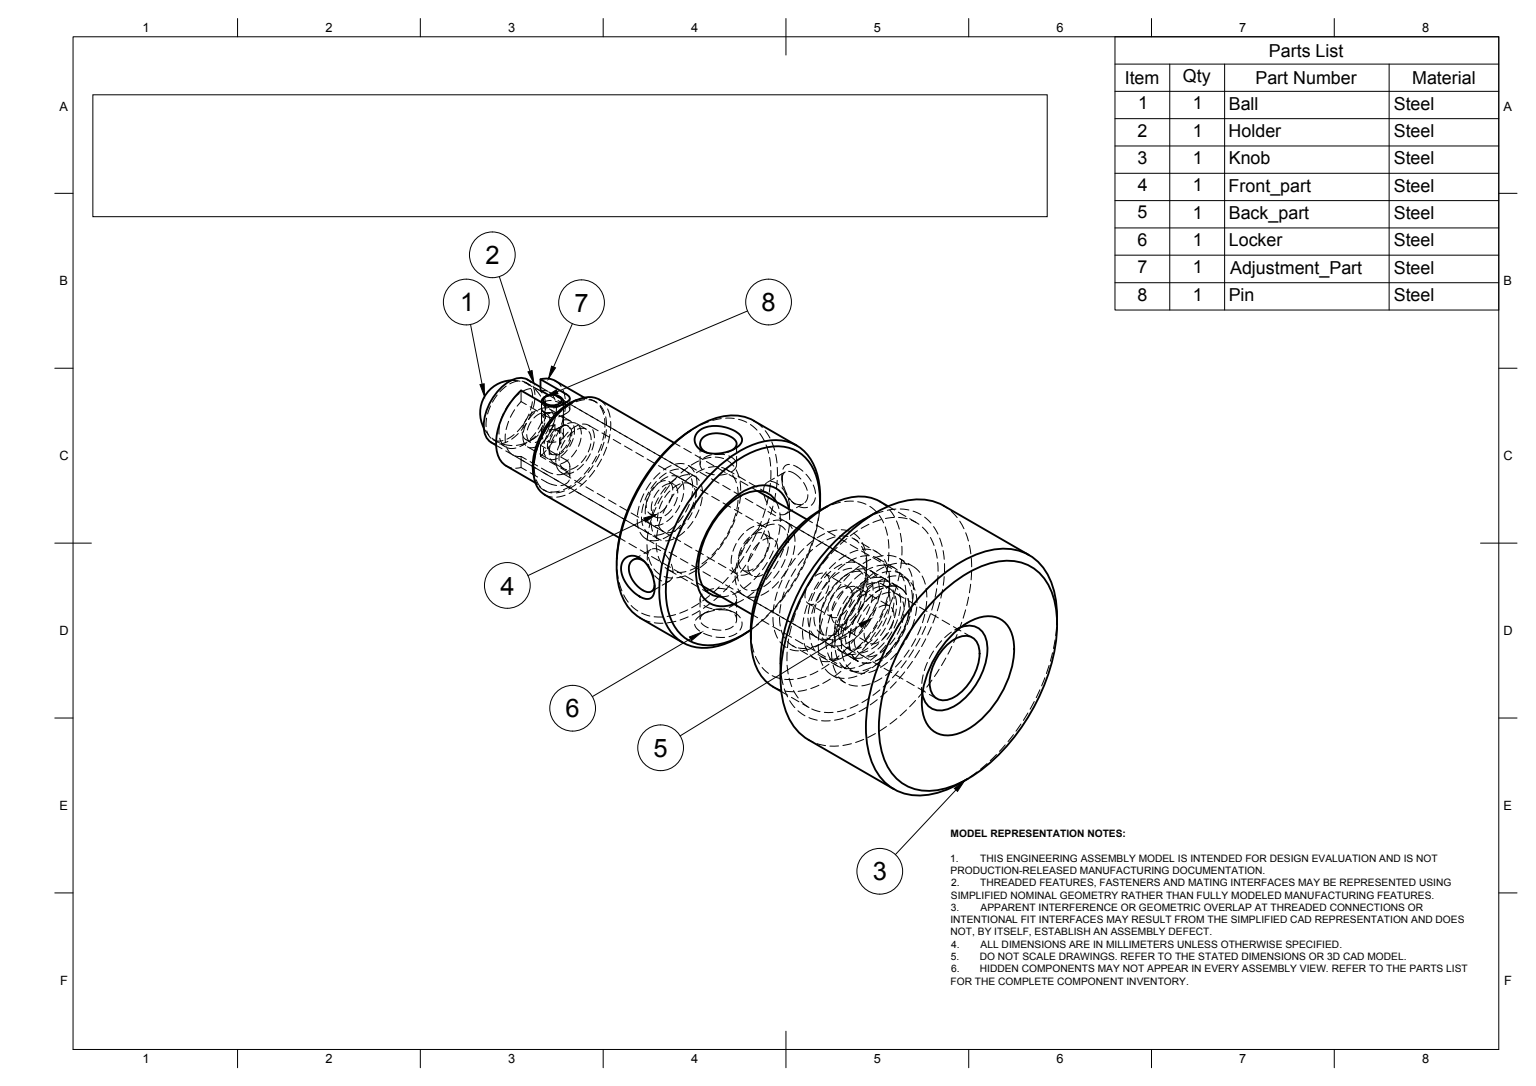
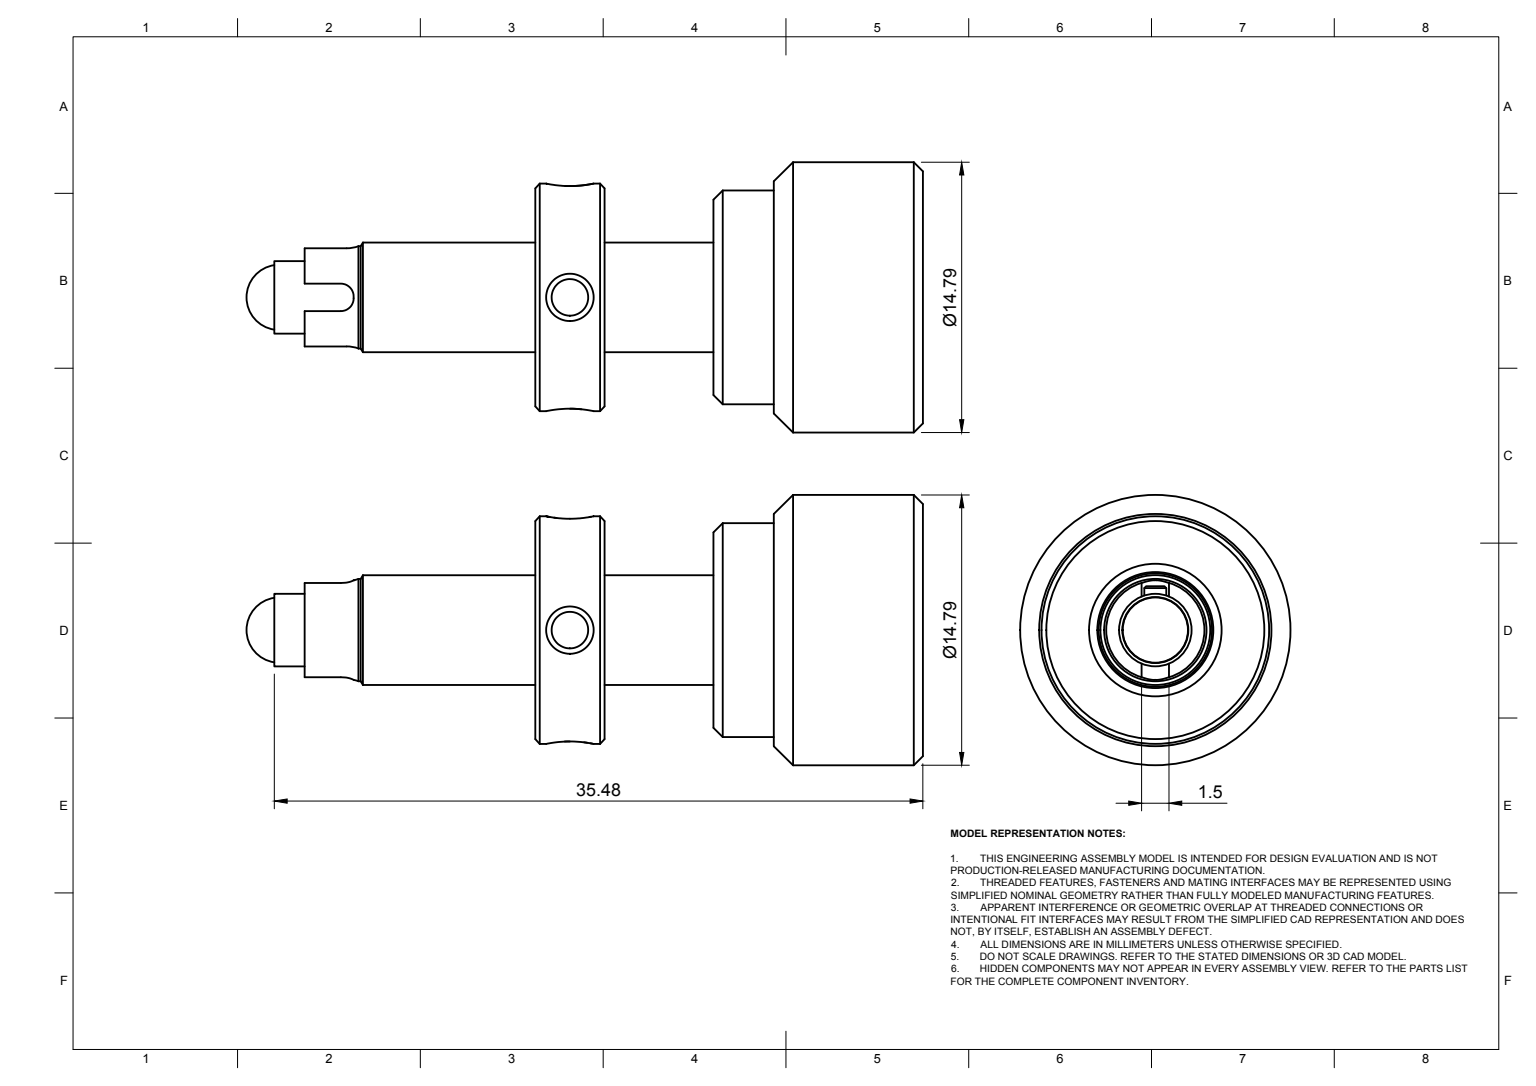
ISO-10303-21;
HEADER;
/* Generated by software containing ST-Developer
 * from STEP Tools, Inc. (www.steptools.com) 
 */

FILE_DESCRIPTION(
/* description */ (''),
/* implementation_level */ '2;1');

FILE_NAME(
/* name */ 'BR-155',
/* time_stamp */ '2026-10-05T00:51:14-07:00',
/* author */ (''),
/* organization */ (''),
/* preprocessor_version */ 'ST-DEVELOPER v20.2',
/* originating_system */ 'Autodesk Translation Framework v15.15.0.0',
/* authorisation */ '');

FILE_SCHEMA (('AUTOMOTIVE_DESIGN { 1 0 10303 214 3 1 1 }'));
ENDSEC;

DATA;
#10=MECHANICAL_DESIGN_GEOMETRIC_PRESENTATION_REPRESENTATION('',(#387,#388,
#389,#390,#391,#392,#393,#394),#4613);
#11=ITEM_DEFINED_TRANSFORMATION($,$,#1692,#1894);
#12=ITEM_DEFINED_TRANSFORMATION($,$,#1695,#1895);
#13=ITEM_DEFINED_TRANSFORMATION($,$,#1728,#1896);
#14=ITEM_DEFINED_TRANSFORMATION($,$,#1765,#1897);
#15=ITEM_DEFINED_TRANSFORMATION($,$,#1791,#1898);
#16=ITEM_DEFINED_TRANSFORMATION($,$,#1812,#1899);
#17=ITEM_DEFINED_TRANSFORMATION($,$,#1841,#1900);
#18=ITEM_DEFINED_TRANSFORMATION($,$,#1886,#1901);
#19=(
REPRESENTATION_RELATIONSHIP($,$,#4645,#4644)
REPRESENTATION_RELATIONSHIP_WITH_TRANSFORMATION(#11)
SHAPE_REPRESENTATION_RELATIONSHIP()
);
#20=(
REPRESENTATION_RELATIONSHIP($,$,#4646,#4644)
REPRESENTATION_RELATIONSHIP_WITH_TRANSFORMATION(#12)
SHAPE_REPRESENTATION_RELATIONSHIP()
);
#21=(
REPRESENTATION_RELATIONSHIP($,$,#4647,#4644)
REPRESENTATION_RELATIONSHIP_WITH_TRANSFORMATION(#13)
SHAPE_REPRESENTATION_RELATIONSHIP()
);
#22=(
REPRESENTATION_RELATIONSHIP($,$,#4648,#4644)
REPRESENTATION_RELATIONSHIP_WITH_TRANSFORMATION(#14)
SHAPE_REPRESENTATION_RELATIONSHIP()
);
#23=(
REPRESENTATION_RELATIONSHIP($,$,#4649,#4644)
REPRESENTATION_RELATIONSHIP_WITH_TRANSFORMATION(#15)
SHAPE_REPRESENTATION_RELATIONSHIP()
);
#24=(
REPRESENTATION_RELATIONSHIP($,$,#4650,#4644)
REPRESENTATION_RELATIONSHIP_WITH_TRANSFORMATION(#16)
SHAPE_REPRESENTATION_RELATIONSHIP()
);
#25=(
REPRESENTATION_RELATIONSHIP($,$,#4651,#4644)
REPRESENTATION_RELATIONSHIP_WITH_TRANSFORMATION(#17)
SHAPE_REPRESENTATION_RELATIONSHIP()
);
#26=(
REPRESENTATION_RELATIONSHIP($,$,#4652,#4644)
REPRESENTATION_RELATIONSHIP_WITH_TRANSFORMATION(#18)
SHAPE_REPRESENTATION_RELATIONSHIP()
);
#27=CONTEXT_DEPENDENT_SHAPE_REPRESENTATION(#19,#4636);
#28=CONTEXT_DEPENDENT_SHAPE_REPRESENTATION(#20,#4637);
#29=CONTEXT_DEPENDENT_SHAPE_REPRESENTATION(#21,#4638);
#30=CONTEXT_DEPENDENT_SHAPE_REPRESENTATION(#22,#4639);
#31=CONTEXT_DEPENDENT_SHAPE_REPRESENTATION(#23,#4640);
#32=CONTEXT_DEPENDENT_SHAPE_REPRESENTATION(#24,#4641);
#33=CONTEXT_DEPENDENT_SHAPE_REPRESENTATION(#25,#4642);
#34=CONTEXT_DEPENDENT_SHAPE_REPRESENTATION(#26,#4643);
#35=NEXT_ASSEMBLY_USAGE_OCCURRENCE('Ball:1','Ball:1','Ball:1',#4654,#4655,
'Ball:1');
#36=NEXT_ASSEMBLY_USAGE_OCCURRENCE('Holder:1','Holder:1','Holder:1',#4654,
#4656,'Holder:1');
#37=NEXT_ASSEMBLY_USAGE_OCCURRENCE('Knob:1','Knob:1','Knob:1',#4654,#4657,
'Knob:1');
#38=NEXT_ASSEMBLY_USAGE_OCCURRENCE('Front_part:1','Front_part:1',
'Front_part:1',#4654,#4658,'Front_part:1');
#39=NEXT_ASSEMBLY_USAGE_OCCURRENCE('Back_part:1','Back_part:1',
'Back_part:1',#4654,#4659,'Back_part:1');
#40=NEXT_ASSEMBLY_USAGE_OCCURRENCE('Locker:1','Locker:1','Locker:1',#4654,
#4660,'Locker:1');
#41=NEXT_ASSEMBLY_USAGE_OCCURRENCE('Adjustment_Part:1',
'Adjustment_Part:1','Adjustment_Part:1',#4654,#4661,'Adjustment_Part:1');
#42=NEXT_ASSEMBLY_USAGE_OCCURRENCE('Pin:1','Pin:1','Pin:1',#4654,#4662,
'Pin:1');
#43=TOROIDAL_SURFACE('',#1858,4.57788729236058,1.89228053659161);
#44=B_SPLINE_SURFACE_WITH_KNOTS('',3,3,((#2717,#2718,#2719,#2720,#2721,
#2722,#2723,#2724,#2725,#2726,#2727,#2728,#2729,#2730,#2731,#2732,#2733,
#2734,#2735,#2736,#2737,#2738,#2739,#2740,#2741,#2742,#2743),(#2744,#2745,
#2746,#2747,#2748,#2749,#2750,#2751,#2752,#2753,#2754,#2755,#2756,#2757,
#2758,#2759,#2760,#2761,#2762,#2763,#2764,#2765,#2766,#2767,#2768,#2769,
#2770),(#2771,#2772,#2773,#2774,#2775,#2776,#2777,#2778,#2779,#2780,#2781,
#2782,#2783,#2784,#2785,#2786,#2787,#2788,#2789,#2790,#2791,#2792,#2793,
#2794,#2795,#2796,#2797),(#2798,#2799,#2800,#2801,#2802,#2803,#2804,#2805,
#2806,#2807,#2808,#2809,#2810,#2811,#2812,#2813,#2814,#2815,#2816,#2817,
#2818,#2819,#2820,#2821,#2822,#2823,#2824)),.UNSPECIFIED.,.F.,.T.,.F.,(4,
4),(4,1,2,1,1,1,2,2,2,2,2,1,1,1,2,2,4),(-9.33776365674593E-5,1.000525980474),
(0.,0.0377394432573701,0.0754788865147403,0.113217461481148,0.150956036447555,
0.188694611413963,0.226433186380371,0.264172629637741,0.301912072895111,
0.339651516152481,0.377390959409851,0.415129534376259,0.452868109342666,
0.490606684309074,0.528345259275481,0.566084702532851,0.603824145790222),
 .UNSPECIFIED.);
#45=B_SPLINE_SURFACE_WITH_KNOTS('',3,3,((#3469,#3470,#3471,#3472,#3473,
#3474,#3475,#3476,#3477,#3478,#3479,#3480,#3481,#3482,#3483,#3484,#3485,
#3486,#3487,#3488,#3489,#3490,#3491,#3492,#3493,#3494,#3495,#3496,#3497),
(#3498,#3499,#3500,#3501,#3502,#3503,#3504,#3505,#3506,#3507,#3508,#3509,
#3510,#3511,#3512,#3513,#3514,#3515,#3516,#3517,#3518,#3519,#3520,#3521,
#3522,#3523,#3524,#3525,#3526),(#3527,#3528,#3529,#3530,#3531,#3532,#3533,
#3534,#3535,#3536,#3537,#3538,#3539,#3540,#3541,#3542,#3543,#3544,#3545,
#3546,#3547,#3548,#3549,#3550,#3551,#3552,#3553,#3554,#3555),(#3556,#3557,
#3558,#3559,#3560,#3561,#3562,#3563,#3564,#3565,#3566,#3567,#3568,#3569,
#3570,#3571,#3572,#3573,#3574,#3575,#3576,#3577,#3578,#3579,#3580,#3581,
#3582,#3583,#3584)),.UNSPECIFIED.,.F.,.T.,.F.,(4,4),(4,1,2,1,2,1,2,2,2,
1,2,1,1,1,1,1,2,2,4),(-0.000295807310057764,1.00205953088178),(0.,0.0377394432573701,
0.0754788865147402,0.113217461481148,0.150956036447555,0.188694611413963,
0.226433186380371,0.264172629637741,0.301912072895111,0.367956098595508,
0.377390959409851,0.415129534376259,0.433998821859462,0.443433465601064,
0.452868109342666,0.490606684309074,0.528345259275481,0.566084702532851,
0.603824145790222),.UNSPECIFIED.);
#46=B_SPLINE_SURFACE_WITH_KNOTS('',3,3,((#3828,#3829,#3830,#3831,#3832,
#3833,#3834,#3835,#3836,#3837,#3838,#3839,#3840,#3841,#3842,#3843,#3844,
#3845,#3846,#3847,#3848,#3849,#3850,#3851,#3852,#3853,#3854),(#3855,#3856,
#3857,#3858,#3859,#3860,#3861,#3862,#3863,#3864,#3865,#3866,#3867,#3868,
#3869,#3870,#3871,#3872,#3873,#3874,#3875,#3876,#3877,#3878,#3879,#3880,
#3881),(#3882,#3883,#3884,#3885,#3886,#3887,#3888,#3889,#3890,#3891,#3892,
#3893,#3894,#3895,#3896,#3897,#3898,#3899,#3900,#3901,#3902,#3903,#3904,
#3905,#3906,#3907,#3908),(#3909,#3910,#3911,#3912,#3913,#3914,#3915,#3916,
#3917,#3918,#3919,#3920,#3921,#3922,#3923,#3924,#3925,#3926,#3927,#3928,
#3929,#3930,#3931,#3932,#3933,#3934,#3935)),.UNSPECIFIED.,.F.,.T.,.F.,(4,
4),(4,1,2,1,1,1,1,2,2,1,1,2,1,1,2,2,2,4),(-0.000127845078603306,1.00073508349094),
(0.,0.0377394432573701,0.0754788865147403,0.113217461481148,0.150956036447555,
0.160390680189157,0.188694611413963,0.226433186380371,0.264172629637741,
0.292477212080768,0.320781794523796,0.377390959409851,0.405694890634657,
0.433998821859462,0.490606684309074,0.528345259275481,0.566084702532852,
0.603824145790222),.UNSPECIFIED.);
#47=B_SPLINE_SURFACE_WITH_KNOTS('',3,3,((#4130,#4131,#4132,#4133,#4134,
#4135,#4136,#4137,#4138,#4139,#4140,#4141,#4142,#4143,#4144,#4145,#4146,
#4147,#4148,#4149,#4150,#4151,#4152,#4153,#4154,#4155,#4156,#4157,#4158,
#4159),(#4160,#4161,#4162,#4163,#4164,#4165,#4166,#4167,#4168,#4169,#4170,
#4171,#4172,#4173,#4174,#4175,#4176,#4177,#4178,#4179,#4180,#4181,#4182,
#4183,#4184,#4185,#4186,#4187,#4188,#4189),(#4190,#4191,#4192,#4193,#4194,
#4195,#4196,#4197,#4198,#4199,#4200,#4201,#4202,#4203,#4204,#4205,#4206,
#4207,#4208,#4209,#4210,#4211,#4212,#4213,#4214,#4215,#4216,#4217,#4218,
#4219),(#4220,#4221,#4222,#4223,#4224,#4225,#4226,#4227,#4228,#4229,#4230,
#4231,#4232,#4233,#4234,#4235,#4236,#4237,#4238,#4239,#4240,#4241,#4242,
#4243,#4244,#4245,#4246,#4247,#4248,#4249)),.UNSPECIFIED.,.F.,.T.,.F.,(4,
4),(4,1,2,1,2,1,2,2,2,2,2,1,1,1,2,2,2,4),(-9.8278797788155E-5,1.00068681548426),
(0.,0.0377394432573701,0.0754788865147402,0.113217461481148,0.150956036447555,
0.188694611413963,0.226433186380371,0.264172629637741,0.301912072895111,
0.339651516152481,0.377390959409851,0.412770873440858,0.433998821859462,
0.462302753084268,0.490606684309074,0.528345259275481,0.566084702532851,
0.603824145790222),.UNSPECIFIED.);
#48=CONICAL_SURFACE('',#1711,1.35128847266969,0.789744339373133);
#49=CONICAL_SURFACE('',#1732,7.1427431617401,0.785398163397448);
#50=CONICAL_SURFACE('',#1736,3.05686141031491,0.78225893919059);
#51=CONICAL_SURFACE('',#1750,3.23679059459596,0.791003251258806);
#52=CONICAL_SURFACE('',#1754,3.5004929560726,0.791003251258806);
#53=CONICAL_SURFACE('',#1758,5.5976024439511,0.779793075536092);
#54=CONICAL_SURFACE('',#1764,6.87169679329977,0.779793075536091);
#55=CONICAL_SURFACE('',#1766,1.32430878211522,1.03823317791294);
#56=CONICAL_SURFACE('',#1773,2.15547938178353,1.07831899445638);
#57=CONICAL_SURFACE('',#1777,2.17072351166958,1.04154954596305);
#58=CONICAL_SURFACE('',#1792,2.1899902410121,0.823106104053138);
#59=CONICAL_SURFACE('',#1807,1.54725736664436,1.55720056407458);
#60=CONICAL_SURFACE('',#1831,6.09377868362497,0.82078898923398);
#61=CONICAL_SURFACE('',#1832,6.09377868362497,0.82078898923398);
#62=CONICAL_SURFACE('',#1836,3.39812786153974,1.04516253667508);
#63=CONICAL_SURFACE('',#1840,3.39812786153974,1.04516253667508);
#64=CONICAL_SURFACE('',#1877,2.89950556638236,1.03144708645266);
#65=CONICAL_SURFACE('',#1881,2.96124530227324,0.181516066311168);
#66=CONICAL_SURFACE('',#1887,0.550000000000002,0.785398163397437);
#67=FACE_BOUND('',#517,.T.);
#68=FACE_BOUND('',#522,.T.);
#69=FACE_BOUND('',#525,.T.);
#70=FACE_BOUND('',#528,.T.);
#71=FACE_BOUND('',#534,.T.);
#72=FACE_BOUND('',#537,.T.);
#73=FACE_BOUND('',#540,.T.);
#74=FACE_BOUND('',#543,.T.);
#75=FACE_BOUND('',#549,.T.);
#76=FACE_BOUND('',#553,.T.);
#77=FACE_BOUND('',#558,.T.);
#78=FACE_BOUND('',#563,.T.);
#79=FACE_BOUND('',#569,.T.);
#80=FACE_BOUND('',#574,.T.);
#81=FACE_BOUND('',#577,.T.);
#82=FACE_BOUND('',#580,.T.);
#83=FACE_BOUND('',#584,.T.);
#84=FACE_BOUND('',#587,.T.);
#85=FACE_BOUND('',#588,.T.);
#86=FACE_BOUND('',#589,.T.);
#87=FACE_BOUND('',#602,.T.);
#88=FACE_BOUND('',#606,.T.);
#89=FACE_BOUND('',#627,.T.);
#90=FACE_BOUND('',#633,.T.);
#91=PLANE('',#1698);
#92=PLANE('',#1702);
#93=PLANE('',#1706);
#94=PLANE('',#1707);
#95=PLANE('',#1715);
#96=PLANE('',#1719);
#97=PLANE('',#1723);
#98=PLANE('',#1727);
#99=PLANE('',#1734);
#100=PLANE('',#1738);
#101=PLANE('',#1742);
#102=PLANE('',#1746);
#103=PLANE('',#1756);
#104=PLANE('',#1762);
#105=PLANE('',#1771);
#106=PLANE('',#1779);
#107=PLANE('',#1783);
#108=PLANE('',#1784);
#109=PLANE('',#1788);
#110=PLANE('',#1797);
#111=PLANE('',#1801);
#112=PLANE('',#1805);
#113=PLANE('',#1811);
#114=PLANE('',#1822);
#115=PLANE('',#1823);
#116=PLANE('',#1824);
#117=PLANE('',#1827);
#118=PLANE('',#1828);
#119=PLANE('',#1834);
#120=PLANE('',#1842);
#121=PLANE('',#1843);
#122=PLANE('',#1845);
#123=PLANE('',#1848);
#124=PLANE('',#1850);
#125=PLANE('',#1852);
#126=PLANE('',#1871);
#127=PLANE('',#1872);
#128=PLANE('',#1873);
#129=PLANE('',#1883);
#130=PLANE('',#1892);
#131=PLANE('',#1893);
#132=B_SPLINE_CURVE_WITH_KNOTS('',3,(#2423,#2424,#2425,#2426,#2427,#2428),
 .UNSPECIFIED.,.F.,.F.,(4,2,4),(0.0611341523507192,0.0707646671678304,0.089396591469994),
 .UNSPECIFIED.);
#133=B_SPLINE_CURVE_WITH_KNOTS('',3,(#2432,#2433,#2434,#2435,#2436,#2437,
#2438,#2439,#2440,#2441,#2442,#2443,#2444,#2445,#2446,#2447,#2448),
 .UNSPECIFIED.,.F.,.F.,(4,2,2,2,3,2,2,4),(-0.0922607888499982,-0.0692273118115021,
-0.0461938347730059,-0.023096917386503,0.,0.023096917386503,0.0461938347730059,
0.0596041129805193),.UNSPECIFIED.);
#134=B_SPLINE_CURVE_WITH_KNOTS('',3,(#2452,#2453,#2454,#2455,#2456,#2457,
#2458,#2459,#2460,#2461),.UNSPECIFIED.,.F.,.F.,(4,2,2,2,4),(0.,0.0227593204764388,
0.0455186409528775,0.0682709506447675,0.0910232603366575),.UNSPECIFIED.);
#135=B_SPLINE_CURVE_WITH_KNOTS('',3,(#2463,#2464,#2465,#2466,#2467,#2468,
#2469,#2470,#2471,#2472),.UNSPECIFIED.,.F.,.F.,(4,2,2,2,4),(0.273069781009973,
0.295822090701863,0.318574400393753,0.341333720870191,0.36409304134663),
 .UNSPECIFIED.);
#136=B_SPLINE_CURVE_WITH_KNOTS('',3,(#2473,#2474,#2475,#2476,#2477,#2478,
#2479,#2480,#2481,#2482,#2483,#2484,#2485,#2486,#2487,#2488,#2489,#2490),
 .UNSPECIFIED.,.F.,.F.,(4,2,2,2,2,2,2,2,4),(0.0910232603366575,0.113775570028548,
0.136527879720438,0.159287200196876,0.182046520673315,0.204805841149754,
0.227565161626193,0.250317471318083,0.273069781009973),.UNSPECIFIED.);
#137=B_SPLINE_CURVE_WITH_KNOTS('',3,(#2492,#2493,#2494,#2495,#2496,#2497,
#2498,#2499,#2500,#2501,#2502,#2503,#2504,#2505,#2506,#2507),
 .UNSPECIFIED.,.F.,.F.,(4,2,2,2,2,2,2,4),(-0.244125690634136,-0.230715412473002,
-0.207618495086499,-0.184521577699996,-0.161424660313493,-0.13832774292699,
-0.115294265888494,-0.0922607888499982),.UNSPECIFIED.);
#138=B_SPLINE_CURVE_WITH_KNOTS('',3,(#2510,#2511,#2512,#2513,#2514,#2515),
 .UNSPECIFIED.,.F.,.F.,(4,2,4),(0.0989596757247573,0.117591600026921,0.127222114844032),
 .UNSPECIFIED.);
#139=B_SPLINE_CURVE_WITH_KNOTS('',3,(#2829,#2830,#2831,#2832,#2833,#2834,
#2835,#2836,#2837,#2838,#2839,#2840,#2841,#2842,#2843,#2844,#2845,#2846,
#2847,#2848,#2849,#2850,#2851,#2852,#2853,#2854,#2855,#2856,#2857,#2858,
#2859,#2860,#2861,#2862,#2863,#2864,#2865,#2866,#2867,#2868,#2869,#2870,
#2871,#2872,#2873,#2874,#2875,#2876,#2877,#2878,#2879,#2880,#2881,#2882,
#2883,#2884,#2885,#2886),.UNSPECIFIED.,.F.,.F.,(4,3,3,3,3,3,3,3,3,3,3,3,
3,3,3,3,3,3,3,4),(0.,0.00830256342986541,0.0165421526797814,0.024758238338255,
0.0329694780959283,0.0377394432573701,0.0461457227075515,0.0546067113015583,
0.063111349941413,0.0717202621168138,0.0754788865147403,0.0836526270820083,
0.0917610027075096,0.0998510566328465,0.107954786491979,0.113217461481148,
0.124926744470172,0.136958735315253,0.149276745375588,0.150956036447555),
 .UNSPECIFIED.);
#140=B_SPLINE_CURVE_WITH_KNOTS('',3,(#2887,#2888,#2889,#2890,#2891,#2892,
#2893,#2894,#2895,#2896,#2897,#2898,#2899,#2900,#2901,#2902,#2903,#2904,
#2905,#2906,#2907,#2908),.UNSPECIFIED.,.F.,.F.,(4,1,2,2,2,2,2,1,1,1,2,2,
4),(0.150956036447555,0.188694611413963,0.226433186380371,0.264172629637741,
0.301912072895111,0.339651516152481,0.377390959409851,0.415129534376259,
0.452868109342666,0.490606684309074,0.528345259275481,0.566084702532851,
0.603824145790222),.UNSPECIFIED.);
#141=B_SPLINE_CURVE_WITH_KNOTS('',3,(#2910,#2911,#2912,#2913,#2914,#2915,
#2916,#2917,#2918,#2919,#2920,#2921,#2922,#2923,#2924,#2925,#2926,#2927),
 .UNSPECIFIED.,.F.,.F.,(4,2,2,2,2,2,2,2,4),(0.,0.0225535375719625,0.045742561528813,
0.0614467959049737,0.0822737875323286,0.105553304717535,0.131394096503778,
0.166373424514803,0.179386291539105),.UNSPECIFIED.);
#142=B_SPLINE_CURVE_WITH_KNOTS('',3,(#2929,#2930,#2931,#2932,#2933,#2934,
#2935,#2936,#2937,#2938,#2939,#2940,#2941,#2942,#2943,#2944,#2945,#2946,
#2947,#2948,#2949,#2950,#2951,#2952,#2953,#2954,#2955,#2956,#2957,#2958,
#2959,#2960),.UNSPECIFIED.,.F.,.F.,(4,2,2,2,2,2,2,2,2,2,2,2,2,2,2,4),(0.179386291539105,
0.180187796446041,0.193753938234979,0.227654303126555,0.255593035139534,
0.354710269922964,0.40331380346349,0.454831190769845,0.497871745499511,
0.537911247906565,0.557044545701239,0.596336621939663,0.650672125427441,
0.738536442549073,0.86973485948851,1.00167935296521),.UNSPECIFIED.);
#143=B_SPLINE_CURVE_WITH_KNOTS('',3,(#2961,#2962,#2963,#2964,#2965,#2966,
#2967,#2968,#2969,#2970,#2971,#2972,#2973,#2974),.UNSPECIFIED.,.F.,.F.,
(4,2,2,2,2,2,4),(2.12484122892953E-5,0.0384114166919255,0.0840005064200764,
0.134083217100535,0.322530315130806,0.421641395496061,0.518312663440211),
 .UNSPECIFIED.);
#144=B_SPLINE_CURVE_WITH_KNOTS('',3,(#2983,#2984,#2985,#2986,#2987,#2988,
#2989,#2990,#2991,#2992,#2993,#2994,#2995,#2996,#2997,#2998,#2999,#3000,
#3001,#3002,#3003,#3004,#3005,#3006,#3007,#3008,#3009,#3010,#3011,#3012,
#3013,#3014,#3015,#3016,#3017,#3018,#3019,#3020,#3021,#3022,#3023,#3024,
#3025,#3026,#3027,#3028,#3029,#3030,#3031,#3032,#3033,#3034,#3035,#3036,
#3037,#3038,#3039,#3040,#3041,#3042,#3043,#3044,#3045,#3046,#3047,#3048,
#3049,#3050,#3051,#3052,#3053,#3054,#3055,#3056,#3057,#3058,#3059,#3060,
#3061,#3062,#3063,#3064,#3065,#3066,#3067,#3068,#3069,#3070,#3071,#3072,
#3073,#3074,#3075,#3076,#3077,#3078,#3079,#3080,#3081,#3082,#3083,#3084,
#3085,#3086,#3087,#3088,#3089,#3090,#3091,#3092,#3093,#3094,#3095,#3096,
#3097,#3098,#3099,#3100,#3101,#3102,#3103,#3104,#3105,#3106,#3107,#3108,
#3109,#3110,#3111,#3112,#3113,#3114,#3115,#3116,#3117,#3118,#3119,#3120,
#3121,#3122,#3123,#3124,#3125,#3126,#3127,#3128,#3129,#3130,#3131,#3132,
#3133,#3134,#3135,#3136,#3137,#3138,#3139,#3140,#3141,#3142,#3143,#3144,
#3145,#3146,#3147,#3148),.UNSPECIFIED.,.T.,.F.,(4,3,3,3,3,3,3,3,3,3,3,3,
3,3,3,3,3,3,3,3,3,3,3,3,3,3,3,3,3,3,3,3,3,3,3,3,3,3,3,3,3,3,3,3,3,3,3,3,
3,3,3,3,3,3,3,4),(-0.603824145790222,-0.590391584697042,-0.577063699872746,
-0.566084702532851,-0.547214980904166,-0.533196018247437,-0.528345259275481,
-0.514141540772843,-0.5016291634541,-0.490606684309074,-0.479313082523423,
-0.468129273627917,-0.456937255878014,-0.452868109342666,-0.44488880016883,
-0.443433465601064,-0.43506567000572,-0.433998821859462,-0.422340513015576,
-0.415129534376259,-0.402742107601763,-0.388956278039157,-0.377390959409851,
-0.368495774245557,-0.367956098595508,-0.35039657661204,-0.334829325286879,
-0.320458700988321,-0.307238340240676,-0.301912072895111,-0.288351696410483,
-0.275229547002117,-0.264172629637741,-0.245302908009056,-0.231165617978299,
-0.226433186380371,-0.211738883366401,-0.19886806654317,-0.188694611413963,
-0.177840892685696,-0.167083403070668,-0.156287372800931,-0.150956036447555,
-0.140167573510221,-0.129416044354867,-0.118538583805277,-0.113217461481148,
-0.100521490014891,-0.0863362768838805,-0.0754788865147402,-0.0614072540763898,
-0.0441325663214528,-0.0377394432573701,-0.0243206710161803,-0.0108972336665805,
0.),.UNSPECIFIED.);
#145=B_SPLINE_CURVE_WITH_KNOTS('',3,(#3150,#3151,#3152,#3153,#3154,#3155,
#3156,#3157,#3158,#3159,#3160,#3161,#3162,#3163,#3164,#3165,#3166,#3167,
#3168,#3169,#3170,#3171,#3172,#3173,#3174,#3175,#3176,#3177,#3178,#3179,
#3180,#3181,#3182,#3183,#3184,#3185,#3186,#3187,#3188,#3189,#3190,#3191,
#3192,#3193,#3194,#3195,#3196,#3197,#3198,#3199,#3200,#3201,#3202,#3203,
#3204,#3205,#3206,#3207,#3208,#3209,#3210,#3211,#3212,#3213,#3214,#3215,
#3216,#3217,#3218,#3219,#3220,#3221,#3222,#3223,#3224,#3225,#3226,#3227,
#3228,#3229,#3230,#3231,#3232,#3233,#3234,#3235,#3236,#3237,#3238,#3239,
#3240,#3241,#3242,#3243,#3244,#3245,#3246,#3247,#3248,#3249,#3250,#3251,
#3252,#3253,#3254,#3255,#3256,#3257,#3258,#3259,#3260,#3261,#3262,#3263,
#3264,#3265,#3266,#3267,#3268,#3269,#3270,#3271,#3272,#3273,#3274,#3275,
#3276,#3277,#3278,#3279,#3280,#3281,#3282,#3283,#3284,#3285,#3286,#3287,
#3288,#3289,#3290,#3291,#3292,#3293,#3294,#3295,#3296,#3297,#3298,#3299,
#3300,#3301,#3302,#3303,#3304,#3305,#3306),.UNSPECIFIED.,.T.,.F.,(4,3,3,
3,3,3,3,3,3,3,3,3,3,3,3,3,3,3,3,3,3,3,3,3,3,3,3,3,3,3,3,3,3,3,3,3,3,3,3,
3,3,3,3,3,3,3,3,3,3,3,3,3,4),(-0.603824145790222,-0.59040484149205,-0.577046286087289,
-0.566084702532851,-0.547214980904166,-0.533215939038458,-0.528345259275481,
-0.513405700683712,-0.500371614295665,-0.490606684309074,-0.479523112948318,
-0.468575947550825,-0.462302753084268,-0.448150787471865,-0.433998821859462,
-0.424198693428956,-0.414259352480831,-0.412770873440858,-0.398547629668401,
-0.382168241492649,-0.377390959409851,-0.363265067662413,-0.345806810116418,
-0.339651516152481,-0.326317147459025,-0.312908174453228,-0.301912072895111,
-0.288487301763661,-0.2751501468201,-0.264172629637741,-0.245302908009056,
-0.231228232357298,-0.226433186380371,-0.2117347177624,-0.198863361209748,
-0.188694611413963,-0.177846084312265,-0.167093676385978,-0.15630237051341,
-0.150956036447555,-0.140168989421454,-0.129419180679109,-0.118543795278154,
-0.113217461481148,-0.10052665633752,-0.0863472586539609,-0.0754788865147402,
-0.0614129693111486,-0.0441577717811917,-0.0377394432573701,-0.0243211983180093,
-0.0108969351998749,0.),.UNSPECIFIED.);
#146=B_SPLINE_CURVE_WITH_KNOTS('',3,(#3308,#3309,#3310,#3311,#3312,#3313,
#3314,#3315,#3316,#3317,#3318,#3319,#3320,#3321,#3322,#3323,#3324,#3325,
#3326,#3327,#3328,#3329,#3330,#3331,#3332,#3333,#3334,#3335,#3336,#3337,
#3338,#3339,#3340,#3341,#3342,#3343,#3344,#3345,#3346,#3347,#3348,#3349,
#3350,#3351,#3352,#3353,#3354,#3355,#3356,#3357,#3358,#3359,#3360,#3361,
#3362,#3363,#3364,#3365,#3366,#3367,#3368,#3369,#3370,#3371,#3372,#3373,
#3374,#3375,#3376,#3377,#3378,#3379,#3380,#3381,#3382,#3383,#3384,#3385,
#3386,#3387,#3388,#3389,#3390,#3391,#3392,#3393,#3394,#3395,#3396,#3397,
#3398,#3399,#3400,#3401,#3402,#3403,#3404,#3405,#3406,#3407,#3408,#3409,
#3410,#3411,#3412,#3413,#3414,#3415,#3416,#3417,#3418,#3419,#3420,#3421,
#3422,#3423,#3424,#3425,#3426,#3427,#3428,#3429,#3430,#3431,#3432,#3433,
#3434,#3435,#3436,#3437,#3438,#3439,#3440,#3441,#3442,#3443,#3444,#3445,
#3446,#3447,#3448,#3449,#3450,#3451,#3452,#3453,#3454,#3455,#3456,#3457,
#3458,#3459,#3460,#3461,#3462,#3463,#3464),.UNSPECIFIED.,.T.,.F.,(4,3,3,
3,3,3,3,3,3,3,3,3,3,3,3,3,3,3,3,3,3,3,3,3,3,3,3,3,3,3,3,3,3,3,3,3,3,3,3,
3,3,3,3,3,3,3,3,3,3,3,3,3,4),(-0.603824145790222,-0.590411465612469,-0.577041801624018,
-0.566084702532852,-0.547214980904167,-0.533151553554515,-0.528345259275481,
-0.511854870778258,-0.497832584846173,-0.490606684309074,-0.473210539692822,
-0.455925683856001,-0.438701796249427,-0.433998821859462,-0.423201659387045,
-0.412132127313061,-0.405694890634657,-0.390813405226797,-0.377390959409851,
-0.359294156561789,-0.340037975542793,-0.32497088632671,-0.320781794523796,
-0.307843399048729,-0.294273409598876,-0.292477212080768,-0.279144117317815,
-0.266288363724764,-0.264172629637741,-0.245302908009056,-0.231166470585065,
-0.226433186380371,-0.210823746419028,-0.197307415534654,-0.188694611413963,
-0.178396491003475,-0.168205689857489,-0.160390680189157,-0.15167832823336,
-0.150956036447555,-0.139587056809165,-0.128218450390218,-0.116689538696443,
-0.113217461481148,-0.100992605061081,-0.0874389990760216,-0.0754788865147403,
-0.0614233370420267,-0.0442069385936118,-0.0377394432573701,-0.0243181691647032,
-0.010894129954878,0.),.UNSPECIFIED.);
#147=B_SPLINE_CURVE_WITH_KNOTS('',3,(#3588,#3589,#3590,#3591,#3592,#3593,
#3594,#3595,#3596,#3597,#3598,#3599,#3600,#3601,#3602,#3603,#3604,#3605,
#3606,#3607,#3608,#3609,#3610,#3611,#3612,#3613,#3614,#3615,#3616,#3617,
#3618,#3619,#3620,#3621,#3622,#3623,#3624,#3625,#3626,#3627,#3628,#3629,
#3630,#3631,#3632,#3633,#3634,#3635,#3636,#3637,#3638,#3639,#3640,#3641,
#3642,#3643,#3644,#3645),.UNSPECIFIED.,.F.,.F.,(4,3,3,3,3,3,3,3,3,3,3,3,
3,3,3,3,3,3,3,4),(0.,0.00829573762667763,0.0165281897599753,0.0247370376512881,
0.0329409858379027,0.0377394432573701,0.0462233213317535,0.0547599525540828,
0.0633384602639499,0.0720158188648333,0.0754788865147402,0.0849135302563422,
0.0940108607641121,0.103092592101262,0.112175512163797,0.113217461481148,
0.122710740047244,0.132228579300877,0.141826740872809,0.150956036447555),
 .UNSPECIFIED.);
#148=B_SPLINE_CURVE_WITH_KNOTS('',3,(#3646,#3647,#3648,#3649,#3650,#3651,
#3652,#3653,#3654,#3655,#3656,#3657,#3658,#3659,#3660,#3661,#3662,#3663,
#3664,#3665,#3666,#3667,#3668,#3669,#3670,#3671,#3672,#3673,#3674,#3675,
#3676,#3677,#3678,#3679,#3680,#3681,#3682,#3683,#3684,#3685,#3686,#3687,
#3688,#3689,#3690,#3691,#3692,#3693,#3694,#3695,#3696,#3697,#3698,#3699,
#3700,#3701,#3702,#3703,#3704,#3705,#3706,#3707,#3708,#3709,#3710,#3711,
#3712,#3713,#3714,#3715,#3716,#3717,#3718,#3719,#3720,#3721,#3722,#3723,
#3724,#3725,#3726,#3727,#3728,#3729,#3730,#3731,#3732,#3733,#3734,#3735,
#3736,#3737,#3738,#3739,#3740,#3741,#3742,#3743,#3744,#3745,#3746,#3747,
#3748,#3749,#3750,#3751,#3752,#3753,#3754,#3755,#3756,#3757,#3758,#3759,
#3760,#3761,#3762,#3763,#3764,#3765,#3766,#3767,#3768,#3769,#3770,#3771,
#3772,#3773,#3774,#3775,#3776,#3777,#3778,#3779,#3780,#3781,#3782,#3783,
#3784,#3785,#3786,#3787,#3788,#3789,#3790,#3791,#3792,#3793,#3794,#3795,
#3796,#3797,#3798,#3799,#3800,#3801,#3802,#3803,#3804,#3805,#3806,#3807,
#3808,#3809,#3810,#3811,#3812,#3813,#3814,#3815,#3816,#3817,#3818,#3819,
#3820,#3821,#3822,#3823),.UNSPECIFIED.,.F.,.F.,(4,3,3,3,3,3,3,3,3,3,3,3,
3,3,3,3,3,3,3,3,3,3,3,3,3,3,3,3,3,3,3,3,3,3,3,3,3,3,3,3,3,3,3,3,3,3,3,3,
3,3,3,3,3,3,3,3,3,3,3,4),(0.150956036447555,0.160549363754181,0.170087496495515,
0.17957549259755,0.188694611413963,0.198129255155565,0.20721232152291,0.216307090036003,
0.225442296384496,0.226433186380371,0.235263130335913,0.243982144413462,
0.252652316208085,0.261280881376461,0.264172629637741,0.272628973289914,
0.281096319050457,0.289577868539869,0.298109252272672,0.301912072895111,
0.310541878044286,0.3191353238789,0.327707744142598,0.336272944326547,0.344860159102294,
0.35346693169753,0.362137437500319,0.367956098595508,0.375378363711079,
0.377390959409851,0.386825603151453,0.395781405680958,0.404721766264308,
0.413665159126656,0.415129534376259,0.426960243388473,0.433998821859462,
0.440518945174589,0.443433465601064,0.449108910733518,0.452868109342666,
0.463354416125425,0.473794794225623,0.484190742563337,0.490606684309074,
0.499415552802534,0.508224959525105,0.517045112657598,0.525909821728332,
0.528345259275481,0.537116996273335,0.545776074243873,0.554386030522553,
0.562954515301158,0.566084702532851,0.574305585613258,0.582536335557294,
0.590782316872269,0.59908512911533,0.603824145790222),.UNSPECIFIED.);
#149=B_SPLINE_CURVE_WITH_KNOTS('',3,(#3939,#3940,#3941,#3942,#3943,#3944,
#3945,#3946,#3947,#3948,#3949,#3950,#3951,#3952,#3953,#3954,#3955,#3956),
 .UNSPECIFIED.,.F.,.F.,(4,2,2,2,2,2,2,2,4),(-0.157966795349973,-0.134769746245384,
-0.111152103192473,-0.0957393456100155,-0.0764377111352473,-0.0499851580328299,
-0.0372293294602945,-0.0183607331665397,-1.54852585271355E-5),
 .UNSPECIFIED.);
#150=B_SPLINE_CURVE_WITH_KNOTS('',3,(#3957,#3958,#3959,#3960,#3961,#3962,
#3963,#3964,#3965,#3966,#3967,#3968,#3969,#3970,#3971,#3972,#3973,#3974,
#3975,#3976,#3977,#3978,#3979,#3980,#3981,#3982,#3983,#3984,#3985,#3986,
#3987,#3988,#3989,#3990,#3991,#3992,#3993,#3994,#3995,#3996,#3997,#3998,
#3999,#4000,#4001,#4002,#4003,#4004,#4005,#4006,#4007,#4008,#4009,#4010,
#4011,#4012,#4013,#4014,#4015,#4016,#4017,#4018,#4019,#4020,#4021,#4022,
#4023,#4024,#4025,#4026,#4027,#4028,#4029,#4030,#4031,#4032,#4033,#4034,
#4035,#4036,#4037,#4038,#4039,#4040,#4041,#4042,#4043,#4044,#4045,#4046,
#4047,#4048,#4049,#4050,#4051,#4052,#4053,#4054,#4055,#4056,#4057,#4058,
#4059,#4060,#4061,#4062,#4063,#4064,#4065,#4066,#4067,#4068,#4069,#4070,
#4071,#4072,#4073,#4074,#4075,#4076,#4077,#4078,#4079,#4080,#4081,#4082,
#4083,#4084,#4085,#4086,#4087,#4088,#4089,#4090,#4091,#4092,#4093,#4094,
#4095,#4096,#4097,#4098,#4099,#4100,#4101,#4102,#4103,#4104,#4105,#4106,
#4107,#4108,#4109,#4110,#4111,#4112,#4113,#4114,#4115,#4116,#4117,#4118,
#4119,#4120,#4121,#4122),.UNSPECIFIED.,.F.,.F.,(4,3,3,3,3,3,3,3,3,3,3,3,
3,3,3,3,3,3,3,3,3,3,3,3,3,3,3,3,3,3,3,3,3,3,3,3,3,3,3,3,3,3,3,3,3,3,3,3,
3,3,3,3,3,3,3,4),(0.150956046102631,0.157057308185334,0.160390680189157,
0.169102327349017,0.177761740636142,0.186381822627463,0.188694611413963,
0.198129255155565,0.207504363975699,0.216968775178035,0.226433186380371,
0.235339806064433,0.244136369675249,0.252883841436447,0.26158882295505,
0.264172629637741,0.273921145643219,0.283689652217834,0.292477212080768,
0.301909496950062,0.311349416446087,0.320781794523796,0.328948709583596,
0.33710056797636,0.345254117291374,0.353452734644994,0.361688284787263,
0.37003334621096,0.377390959409851,0.385901375718853,0.394375368564309,
0.402830843321504,0.405694890634657,0.415170724108714,0.424683263298954,
0.433998821859462,0.443965968418747,0.454061131183995,0.46415325099199,
0.474130092027922,0.483814161418412,0.490606684309074,0.500095510584781,
0.509588520092461,0.519121097655791,0.528345259275481,0.537152260065718,
0.545849424317997,0.554498405743932,0.563106711158609,0.566084702532852,
0.574301473245816,0.582528508095237,0.590771006435055,0.599070784708944,
0.603824145790222),.UNSPECIFIED.);
#151=B_SPLINE_CURVE_WITH_KNOTS('',3,(#4253,#4254,#4255,#4256,#4257,#4258,
#4259,#4260,#4261,#4262,#4263,#4264,#4265,#4266,#4267,#4268,#4269,#4270,
#4271,#4272),.UNSPECIFIED.,.F.,.F.,(4,2,2,2,2,2,2,2,2,4),(-0.63257270273012,
-0.613187885769762,-0.594110099534741,-0.574392662092664,-0.55480528669817,
-0.535546049297075,-0.516021545010237,-0.496492553321205,-0.477063998339651,
-0.474227533561733),.UNSPECIFIED.);
#152=B_SPLINE_CURVE_WITH_KNOTS('',3,(#4273,#4274,#4275,#4276,#4277,#4278,
#4279,#4280,#4281,#4282,#4283,#4284,#4285,#4286,#4287,#4288,#4289,#4290,
#4291,#4292,#4293,#4294,#4295,#4296,#4297,#4298,#4299,#4300,#4301,#4302,
#4303,#4304,#4305,#4306,#4307,#4308,#4309,#4310,#4311,#4312,#4313,#4314,
#4315,#4316,#4317,#4318,#4319,#4320,#4321,#4322,#4323,#4324),
 .UNSPECIFIED.,.F.,.F.,(4,2,2,2,2,2,2,2,2,2,2,2,2,2,2,2,2,2,2,2,2,2,2,2,
2,4),(-0.474227533561733,-0.458329372527362,-0.439173439486182,-0.419731155843369,
-0.400140639763559,-0.381254494509653,-0.362129574615996,-0.342849277390761,
-0.315940533098414,-0.289017768986139,-0.269733478910581,-0.250586364422205,
-0.231653812692583,-0.21172855838034,-0.201929598171686,-0.182564500685825,
-0.163995370742465,-0.144570150007686,-0.125002244985411,-0.105396599383871,
-0.0956567919090896,-0.0764809925540918,-0.0569765610843296,-0.0373737466489288,
-0.0184652873791742,0.),.UNSPECIFIED.);
#153=B_SPLINE_CURVE_WITH_KNOTS('',3,(#4375,#4376,#4377,#4378,#4379,#4380),
 .UNSPECIFIED.,.F.,.F.,(4,2,4),(0.,0.0265093466366244,0.0315326488828016),
 .UNSPECIFIED.);
#154=B_SPLINE_CURVE_WITH_KNOTS('',3,(#4382,#4383,#4384,#4385,#4386,#4387,
#4388,#4389,#4390,#4391),.UNSPECIFIED.,.F.,.F.,(4,2,2,2,4),(-0.106715130399001,
-0.0799992414062105,-0.0532833524134197,-0.0266416762067098,0.),
 .UNSPECIFIED.);
#155=B_SPLINE_CURVE_WITH_KNOTS('',3,(#4394,#4395,#4396,#4397,#4398,#4399,
#4400,#4401,#4402,#4403,#4404,#4405,#4406),.UNSPECIFIED.,.F.,.F.,(4,2,2,
2,3,4),(0.378639974335924,0.39855724329992,0.425776827887283,0.447703205216881,
0.457107149533339,0.457130414187804),.UNSPECIFIED.);
#156=B_SPLINE_CURVE_WITH_KNOTS('',3,(#4424,#4425,#4426,#4427,#4428,#4429,
#4430,#4431,#4432,#4433,#4434,#4435,#4436),.UNSPECIFIED.,.F.,.F.,(4,3,2,
2,2,4),(0.457052713610798,0.457075978112808,0.477097828431014,0.502267294711213,
0.530728459336765,0.53557163395288),.UNSPECIFIED.);
#157=B_SPLINE_CURVE_WITH_KNOTS('',3,(#4437,#4438,#4439,#4440,#4441,#4442,
#4443,#4444,#4445,#4446),.UNSPECIFIED.,.F.,.F.,(4,2,2,2,4),(-0.212983885016079,
-0.186342208809369,-0.159700532602659,-0.132984643609868,-0.106268754617077),
 .UNSPECIFIED.);
#158=B_SPLINE_CURVE_WITH_KNOTS('',3,(#4447,#4448,#4449,#4450,#4451,#4452),
 .UNSPECIFIED.,.F.,.F.,(4,2,4),(0.180491212128822,0.185514514374999,0.212023861011624),
 .UNSPECIFIED.);
#159=B_SPLINE_CURVE_WITH_KNOTS('',3,(#4465,#4466,#4467,#4468,#4469,#4470,
#4471,#4472,#4473,#4474),.UNSPECIFIED.,.F.,.F.,(4,2,2,2,4),(0.152701408415346,
0.169165149472481,0.195857989456366,0.218518872787138,0.230918738867668),
 .UNSPECIFIED.);
#160=B_SPLINE_CURVE_WITH_KNOTS('',3,(#4475,#4476,#4477,#4478,#4479,#4480),
 .UNSPECIFIED.,.F.,.F.,(4,2,4),(0.212023861011624,0.238533207648248,0.243556509894426),
 .UNSPECIFIED.);
#161=B_SPLINE_CURVE_WITH_KNOTS('',3,(#4482,#4483,#4484,#4485,#4486,#4487,
#4488,#4489,#4490,#4491),.UNSPECIFIED.,.F.,.F.,(4,2,2,2,4),(-0.319699015415081,
-0.29298312642229,-0.266267237429499,-0.239625561222789,-0.212983885016079),
 .UNSPECIFIED.);
#162=B_SPLINE_CURVE_WITH_KNOTS('',3,(#4505,#4506,#4507,#4508,#4509,#4510),
 .UNSPECIFIED.,.F.,.F.,(4,2,4),(0.392515073140443,0.39753837538662,0.424047722023245),
 .UNSPECIFIED.);
#163=B_SPLINE_CURVE_WITH_KNOTS('',3,(#4511,#4512,#4513,#4514,#4515,#4516,
#4517,#4518,#4519,#4520),.UNSPECIFIED.,.F.,.F.,(4,2,2,2,4),(0.224352648954622,
0.240815002701601,0.264724046908964,0.293460711591788,0.30255788453281),
 .UNSPECIFIED.);
#164=B_SPLINE_CURVE_WITH_KNOTS('',3,(#4521,#4522,#4523,#4524,#4525,#4526,
#4527,#4528,#4529,#4530),.UNSPECIFIED.,.F.,.F.,(4,2,2,2,4),(-0.425967770032155,
-0.399326093825445,-0.372684417618735,-0.345968528625944,-0.319252639633153),
 .UNSPECIFIED.);
#165=LINE('',#2417,#248);
#166=LINE('',#2421,#249);
#167=LINE('',#2430,#250);
#168=LINE('',#2450,#251);
#169=LINE('',#2509,#252);
#170=LINE('',#2517,#253);
#171=LINE('',#2521,#254);
#172=LINE('',#2534,#255);
#173=LINE('',#2537,#256);
#174=LINE('',#2542,#257);
#175=LINE('',#2549,#258);
#176=LINE('',#2550,#259);
#177=LINE('',#2557,#260);
#178=LINE('',#2564,#261);
#179=LINE('',#2571,#262);
#180=LINE('',#2575,#263);
#181=LINE('',#2583,#264);
#182=LINE('',#2590,#265);
#183=LINE('',#2597,#266);
#184=LINE('',#2604,#267);
#185=LINE('',#2607,#268);
#186=LINE('',#2612,#269);
#187=LINE('',#2615,#270);
#188=LINE('',#2623,#271);
#189=LINE('',#2627,#272);
#190=LINE('',#2632,#273);
#191=LINE('',#2638,#274);
#192=LINE('',#2643,#275);
#193=LINE('',#2650,#276);
#194=LINE('',#2654,#277);
#195=LINE('',#2657,#278);
#196=LINE('',#2665,#279);
#197=LINE('',#2673,#280);
#198=LINE('',#2678,#281);
#199=LINE('',#2684,#282);
#200=LINE('',#2689,#283);
#201=LINE('',#2696,#284);
#202=LINE('',#2703,#285);
#203=LINE('',#2710,#286);
#204=LINE('',#2714,#287);
#205=LINE('',#2827,#288);
#206=LINE('',#2978,#289);
#207=LINE('',#2980,#290);
#208=LINE('',#3468,#291);
#209=LINE('',#3586,#292);
#210=LINE('',#3827,#293);
#211=LINE('',#3937,#294);
#212=LINE('',#4126,#295);
#213=LINE('',#4251,#296);
#214=LINE('',#4328,#297);
#215=LINE('',#4336,#298);
#216=LINE('',#4339,#299);
#217=LINE('',#4347,#300);
#218=LINE('',#4351,#301);
#219=LINE('',#4353,#302);
#220=LINE('',#4358,#303);
#221=LINE('',#4360,#304);
#222=LINE('',#4362,#305);
#223=LINE('',#4363,#306);
#224=LINE('',#4367,#307);
#225=LINE('',#4369,#308);
#226=LINE('',#4371,#309);
#227=LINE('',#4372,#310);
#228=LINE('',#4393,#311);
#229=LINE('',#4412,#312);
#230=LINE('',#4416,#313);
#231=LINE('',#4418,#314);
#232=LINE('',#4420,#315);
#233=LINE('',#4421,#316);
#234=LINE('',#4456,#317);
#235=LINE('',#4458,#318);
#236=LINE('',#4460,#319);
#237=LINE('',#4461,#320);
#238=LINE('',#4492,#321);
#239=LINE('',#4501,#322);
#240=LINE('',#4539,#323);
#241=LINE('',#4555,#324);
#242=LINE('',#4559,#325);
#243=LINE('',#4563,#326);
#244=LINE('',#4566,#327);
#245=LINE('',#4572,#328);
#246=LINE('',#4578,#329);
#247=LINE('',#4582,#330);
#248=VECTOR('',#1914,10.);
#249=VECTOR('',#1917,10.);
#250=VECTOR('',#1918,10.);
#251=VECTOR('',#1919,0.600000000000001);
#252=VECTOR('',#1920,10.);
#253=VECTOR('',#1923,10.);
#254=VECTOR('',#1928,1.19802042656629);
#255=VECTOR('',#1949,0.898903149093028);
#256=VECTOR('',#1952,1.35128847266969);
#257=VECTOR('',#1959,1.80367379624636);
#258=VECTOR('',#1968,1.9840612380693);
#259=VECTOR('',#1969,1.9840612380693);
#260=VECTOR('',#1978,1.49577760563294);
#261=VECTOR('',#1987,1.24385197034191);
#262=VECTOR('',#1996,7.3927431617401);
#263=VECTOR('',#2001,7.1427431617401);
#264=VECTOR('',#2012,3.05686141031491);
#265=VECTOR('',#2021,1.93367516017024);
#266=VECTOR('',#2030,3.68653879426857);
#267=VECTOR('',#2039,3.10163618786504);
#268=VECTOR('',#2042,3.23679059459596);
#269=VECTOR('',#2049,3.37194500132688);
#270=VECTOR('',#2052,3.5004929560726);
#271=VECTOR('',#2063,5.5976024439511);
#272=VECTOR('',#2068,5.84899819199777);
#273=VECTOR('',#2075,6.87169679329977);
#274=VECTOR('',#2082,1.32430878211522);
#275=VECTOR('',#2089,1.15283995859749);
#276=VECTOR('',#2098,2.15547938178353);
#277=VECTOR('',#2103,2.3164003912567);
#278=VECTOR('',#2106,2.17072351166958);
#279=VECTOR('',#2117,0.94209020647254);
#280=VECTOR('',#2128,1.02706997925809);
#281=VECTOR('',#2135,1.49577760563294);
#282=VECTOR('',#2142,2.1899902410121);
#283=VECTOR('',#2149,2.3164003912567);
#284=VECTOR('',#2158,1.99619194538056);
#285=VECTOR('',#2167,2.3164003912567);
#286=VECTOR('',#2176,1.54725736664436);
#287=VECTOR('',#2181,1.16083957311848);
#288=VECTOR('',#2186,10.);
#289=VECTOR('',#2191,6.22506754791384);
#290=VECTOR('',#2192,6.22506754791384);
#291=VECTOR('',#2199,1.);
#292=VECTOR('',#2200,9.99999999999999);
#293=VECTOR('',#2205,1.);
#294=VECTOR('',#2206,10.);
#295=VECTOR('',#2211,1.);
#296=VECTOR('',#2218,10.);
#297=VECTOR('',#2223,1.);
#298=VECTOR('',#2234,6.09377868362497);
#299=VECTOR('',#2237,6.09377868362497);
#300=VECTOR('',#2248,3.39812786153974);
#301=VECTOR('',#2253,3.17127539348974);
#302=VECTOR('',#2256,3.39812786153974);
#303=VECTOR('',#2261,10.);
#304=VECTOR('',#2262,10.);
#305=VECTOR('',#2263,10.);
#306=VECTOR('',#2264,10.);
#307=VECTOR('',#2267,10.);
#308=VECTOR('',#2268,10.);
#309=VECTOR('',#2269,10.);
#310=VECTOR('',#2270,10.);
#311=VECTOR('',#2273,10.);
#312=VECTOR('',#2280,10.);
#313=VECTOR('',#2283,10.);
#314=VECTOR('',#2284,10.);
#315=VECTOR('',#2285,10.);
#316=VECTOR('',#2286,10.);
#317=VECTOR('',#2291,10.);
#318=VECTOR('',#2292,10.);
#319=VECTOR('',#2293,10.);
#320=VECTOR('',#2294,10.);
#321=VECTOR('',#2297,10.);
#322=VECTOR('',#2306,10.);
#323=VECTOR('',#2323,1.9840612380693);
#324=VECTOR('',#2350,2.79839874569029);
#325=VECTOR('',#2355,2.89950556638236);
#326=VECTOR('',#2360,3.00061238707443);
#327=VECTOR('',#2363,2.96124530227324);
#328=VECTOR('',#2372,2.3164003912567);
#329=VECTOR('',#2379,0.550000000000002);
#330=VECTOR('',#2384,0.600000000000001);
#331=CYLINDRICAL_SURFACE('',#1696,0.600000000000001);
#332=CYLINDRICAL_SURFACE('',#1699,1.19802042656629);
#333=CYLINDRICAL_SURFACE('',#1704,0.898903149093028);
#334=CYLINDRICAL_SURFACE('',#1709,0.898903149093028);
#335=CYLINDRICAL_SURFACE('',#1713,1.80367379624636);
#336=CYLINDRICAL_SURFACE('',#1717,1.9840612380693);
#337=CYLINDRICAL_SURFACE('',#1721,1.49577760563294);
#338=CYLINDRICAL_SURFACE('',#1725,1.24385197034191);
#339=CYLINDRICAL_SURFACE('',#1729,7.3927431617401);
#340=CYLINDRICAL_SURFACE('',#1740,1.93367516017024);
#341=CYLINDRICAL_SURFACE('',#1744,3.68653879426857);
#342=CYLINDRICAL_SURFACE('',#1748,3.10163618786504);
#343=CYLINDRICAL_SURFACE('',#1752,3.37194500132688);
#344=CYLINDRICAL_SURFACE('',#1760,5.84899819199777);
#345=CYLINDRICAL_SURFACE('',#1769,1.15283995859749);
#346=CYLINDRICAL_SURFACE('',#1775,2.3164003912567);
#347=CYLINDRICAL_SURFACE('',#1781,0.94209020647254);
#348=CYLINDRICAL_SURFACE('',#1786,1.02706997925809);
#349=CYLINDRICAL_SURFACE('',#1790,1.49577760563294);
#350=CYLINDRICAL_SURFACE('',#1795,2.3164003912567);
#351=CYLINDRICAL_SURFACE('',#1799,1.99619194538056);
#352=CYLINDRICAL_SURFACE('',#1803,2.3164003912567);
#353=CYLINDRICAL_SURFACE('',#1809,1.16083957311848);
#354=CYLINDRICAL_SURFACE('',#1813,6.22506754791384);
#355=CYLINDRICAL_SURFACE('',#1816,1.);
#356=CYLINDRICAL_SURFACE('',#1818,1.);
#357=CYLINDRICAL_SURFACE('',#1820,1.);
#358=CYLINDRICAL_SURFACE('',#1825,1.);
#359=CYLINDRICAL_SURFACE('',#1838,3.17127539348974);
#360=CYLINDRICAL_SURFACE('',#1844,0.699999999999994);
#361=CYLINDRICAL_SURFACE('',#1849,0.699999999999998);
#362=CYLINDRICAL_SURFACE('',#1851,0.699999999999998);
#363=CYLINDRICAL_SURFACE('',#1857,0.699999999999994);
#364=CYLINDRICAL_SURFACE('',#1863,1.9840612380693);
#365=CYLINDRICAL_SURFACE('',#1867,2.68560675576897);
#366=CYLINDRICAL_SURFACE('',#1869,2.68560675576897);
#367=CYLINDRICAL_SURFACE('',#1875,2.79839874569029);
#368=CYLINDRICAL_SURFACE('',#1879,3.00061238707443);
#369=CYLINDRICAL_SURFACE('',#1885,2.3164003912567);
#370=CYLINDRICAL_SURFACE('',#1890,0.600000000000001);
#371=SHAPE_REPRESENTATION_RELATIONSHIP('SRR','None',#4645,#379);
#372=SHAPE_REPRESENTATION_RELATIONSHIP('SRR','None',#4646,#380);
#373=SHAPE_REPRESENTATION_RELATIONSHIP('SRR','None',#4647,#381);
#374=SHAPE_REPRESENTATION_RELATIONSHIP('SRR','None',#4648,#382);
#375=SHAPE_REPRESENTATION_RELATIONSHIP('SRR','None',#4649,#383);
#376=SHAPE_REPRESENTATION_RELATIONSHIP('SRR','None',#4650,#384);
#377=SHAPE_REPRESENTATION_RELATIONSHIP('SRR','None',#4651,#385);
#378=SHAPE_REPRESENTATION_RELATIONSHIP('SRR','None',#4652,#386);
#379=ADVANCED_BREP_SHAPE_REPRESENTATION('',(#395),#4605);
#380=ADVANCED_BREP_SHAPE_REPRESENTATION('',(#396),#4606);
#381=ADVANCED_BREP_SHAPE_REPRESENTATION('',(#397),#4607);
#382=ADVANCED_BREP_SHAPE_REPRESENTATION('',(#398),#4608);
#383=ADVANCED_BREP_SHAPE_REPRESENTATION('',(#399),#4609);
#384=ADVANCED_BREP_SHAPE_REPRESENTATION('',(#400),#4610);
#385=ADVANCED_BREP_SHAPE_REPRESENTATION('',(#401),#4611);
#386=ADVANCED_BREP_SHAPE_REPRESENTATION('',(#402),#4612);
#387=STYLED_ITEM('',(#4694),#395);
#388=STYLED_ITEM('',(#4695),#396);
#389=STYLED_ITEM('',(#4696),#397);
#390=STYLED_ITEM('',(#4695),#398);
#391=STYLED_ITEM('',(#4695),#399);
#392=STYLED_ITEM('',(#4695),#400);
#393=STYLED_ITEM('',(#4695),#401);
#394=STYLED_ITEM('',(#4697),#402);
#395=MANIFOLD_SOLID_BREP('Body1',#1594);
#396=MANIFOLD_SOLID_BREP('Body1',#1595);
#397=MANIFOLD_SOLID_BREP('Body1',#1596);
#398=MANIFOLD_SOLID_BREP('Body1',#1597);
#399=MANIFOLD_SOLID_BREP('Body1',#1598);
#400=MANIFOLD_SOLID_BREP('Body1',#1599);
#401=MANIFOLD_SOLID_BREP('Body1',#1600);
#402=MANIFOLD_SOLID_BREP('Body1',#1601);
#403=FACE_OUTER_BOUND('',#509,.T.);
#404=FACE_OUTER_BOUND('',#510,.T.);
#405=FACE_OUTER_BOUND('',#511,.T.);
#406=FACE_OUTER_BOUND('',#512,.T.);
#407=FACE_OUTER_BOUND('',#513,.T.);
#408=FACE_OUTER_BOUND('',#514,.T.);
#409=FACE_OUTER_BOUND('',#515,.T.);
#410=FACE_OUTER_BOUND('',#516,.T.);
#411=FACE_OUTER_BOUND('',#518,.T.);
#412=FACE_OUTER_BOUND('',#519,.T.);
#413=FACE_OUTER_BOUND('',#520,.T.);
#414=FACE_OUTER_BOUND('',#521,.T.);
#415=FACE_OUTER_BOUND('',#523,.T.);
#416=FACE_OUTER_BOUND('',#524,.T.);
#417=FACE_OUTER_BOUND('',#526,.T.);
#418=FACE_OUTER_BOUND('',#527,.T.);
#419=FACE_OUTER_BOUND('',#529,.T.);
#420=FACE_OUTER_BOUND('',#530,.T.);
#421=FACE_OUTER_BOUND('',#531,.T.);
#422=FACE_OUTER_BOUND('',#532,.T.);
#423=FACE_OUTER_BOUND('',#533,.T.);
#424=FACE_OUTER_BOUND('',#535,.T.);
#425=FACE_OUTER_BOUND('',#536,.T.);
#426=FACE_OUTER_BOUND('',#538,.T.);
#427=FACE_OUTER_BOUND('',#539,.T.);
#428=FACE_OUTER_BOUND('',#541,.T.);
#429=FACE_OUTER_BOUND('',#542,.T.);
#430=FACE_OUTER_BOUND('',#544,.T.);
#431=FACE_OUTER_BOUND('',#545,.T.);
#432=FACE_OUTER_BOUND('',#546,.T.);
#433=FACE_OUTER_BOUND('',#547,.T.);
#434=FACE_OUTER_BOUND('',#548,.T.);
#435=FACE_OUTER_BOUND('',#550,.T.);
#436=FACE_OUTER_BOUND('',#551,.T.);
#437=FACE_OUTER_BOUND('',#552,.T.);
#438=FACE_OUTER_BOUND('',#554,.T.);
#439=FACE_OUTER_BOUND('',#555,.T.);
#440=FACE_OUTER_BOUND('',#556,.T.);
#441=FACE_OUTER_BOUND('',#557,.T.);
#442=FACE_OUTER_BOUND('',#559,.T.);
#443=FACE_OUTER_BOUND('',#560,.T.);
#444=FACE_OUTER_BOUND('',#561,.T.);
#445=FACE_OUTER_BOUND('',#562,.T.);
#446=FACE_OUTER_BOUND('',#564,.T.);
#447=FACE_OUTER_BOUND('',#565,.T.);
#448=FACE_OUTER_BOUND('',#566,.T.);
#449=FACE_OUTER_BOUND('',#567,.T.);
#450=FACE_OUTER_BOUND('',#568,.T.);
#451=FACE_OUTER_BOUND('',#570,.T.);
#452=FACE_OUTER_BOUND('',#571,.T.);
#453=FACE_OUTER_BOUND('',#572,.T.);
#454=FACE_OUTER_BOUND('',#573,.T.);
#455=FACE_OUTER_BOUND('',#575,.T.);
#456=FACE_OUTER_BOUND('',#576,.T.);
#457=FACE_OUTER_BOUND('',#578,.T.);
#458=FACE_OUTER_BOUND('',#579,.T.);
#459=FACE_OUTER_BOUND('',#581,.T.);
#460=FACE_OUTER_BOUND('',#582,.T.);
#461=FACE_OUTER_BOUND('',#583,.T.);
#462=FACE_OUTER_BOUND('',#585,.T.);
#463=FACE_OUTER_BOUND('',#586,.T.);
#464=FACE_OUTER_BOUND('',#590,.T.);
#465=FACE_OUTER_BOUND('',#591,.T.);
#466=FACE_OUTER_BOUND('',#592,.T.);
#467=FACE_OUTER_BOUND('',#593,.T.);
#468=FACE_OUTER_BOUND('',#594,.T.);
#469=FACE_OUTER_BOUND('',#595,.T.);
#470=FACE_OUTER_BOUND('',#596,.T.);
#471=FACE_OUTER_BOUND('',#597,.T.);
#472=FACE_OUTER_BOUND('',#598,.T.);
#473=FACE_OUTER_BOUND('',#599,.T.);
#474=FACE_OUTER_BOUND('',#600,.T.);
#475=FACE_OUTER_BOUND('',#601,.T.);
#476=FACE_OUTER_BOUND('',#603,.T.);
#477=FACE_OUTER_BOUND('',#604,.T.);
#478=FACE_OUTER_BOUND('',#605,.T.);
#479=FACE_OUTER_BOUND('',#607,.T.);
#480=FACE_OUTER_BOUND('',#608,.T.);
#481=FACE_OUTER_BOUND('',#609,.T.);
#482=FACE_OUTER_BOUND('',#610,.T.);
#483=FACE_OUTER_BOUND('',#611,.T.);
#484=FACE_OUTER_BOUND('',#612,.T.);
#485=FACE_OUTER_BOUND('',#613,.T.);
#486=FACE_OUTER_BOUND('',#614,.T.);
#487=FACE_OUTER_BOUND('',#615,.T.);
#488=FACE_OUTER_BOUND('',#616,.T.);
#489=FACE_OUTER_BOUND('',#617,.T.);
#490=FACE_OUTER_BOUND('',#618,.T.);
#491=FACE_OUTER_BOUND('',#619,.T.);
#492=FACE_OUTER_BOUND('',#620,.T.);
#493=FACE_OUTER_BOUND('',#621,.T.);
#494=FACE_OUTER_BOUND('',#622,.T.);
#495=FACE_OUTER_BOUND('',#623,.T.);
#496=FACE_OUTER_BOUND('',#624,.T.);
#497=FACE_OUTER_BOUND('',#625,.T.);
#498=FACE_OUTER_BOUND('',#626,.T.);
#499=FACE_OUTER_BOUND('',#628,.T.);
#500=FACE_OUTER_BOUND('',#629,.T.);
#501=FACE_OUTER_BOUND('',#630,.T.);
#502=FACE_OUTER_BOUND('',#631,.T.);
#503=FACE_OUTER_BOUND('',#632,.T.);
#504=FACE_OUTER_BOUND('',#634,.T.);
#505=FACE_OUTER_BOUND('',#635,.T.);
#506=FACE_OUTER_BOUND('',#636,.T.);
#507=FACE_OUTER_BOUND('',#637,.T.);
#508=FACE_OUTER_BOUND('',#638,.T.);
#509=EDGE_LOOP('',(#1071,#1072));
#510=EDGE_LOOP('',(#1073,#1074,#1075,#1076,#1077,#1078,#1079,#1080,#1081,
#1082,#1083,#1084,#1085,#1086));
#511=EDGE_LOOP('',(#1087,#1088));
#512=EDGE_LOOP('',(#1089,#1090,#1091,#1092,#1093,#1094));
#513=EDGE_LOOP('',(#1095,#1096,#1097,#1098));
#514=EDGE_LOOP('',(#1099,#1100,#1101,#1102));
#515=EDGE_LOOP('',(#1103,#1104,#1105,#1106));
#516=EDGE_LOOP('',(#1107));
#517=EDGE_LOOP('',(#1108));
#518=EDGE_LOOP('',(#1109,#1110,#1111,#1112));
#519=EDGE_LOOP('',(#1113,#1114,#1115,#1116));
#520=EDGE_LOOP('',(#1117,#1118,#1119,#1120));
#521=EDGE_LOOP('',(#1121));
#522=EDGE_LOOP('',(#1122));
#523=EDGE_LOOP('',(#1123,#1124,#1125,#1126,#1127,#1128,#1129,#1130,#1131));
#524=EDGE_LOOP('',(#1132));
#525=EDGE_LOOP('',(#1133));
#526=EDGE_LOOP('',(#1134,#1135,#1136,#1137));
#527=EDGE_LOOP('',(#1138));
#528=EDGE_LOOP('',(#1139));
#529=EDGE_LOOP('',(#1140,#1141,#1142,#1143));
#530=EDGE_LOOP('',(#1144));
#531=EDGE_LOOP('',(#1145,#1146,#1147,#1148));
#532=EDGE_LOOP('',(#1149,#1150,#1151,#1152));
#533=EDGE_LOOP('',(#1153));
#534=EDGE_LOOP('',(#1154));
#535=EDGE_LOOP('',(#1155,#1156,#1157,#1158));
#536=EDGE_LOOP('',(#1159));
#537=EDGE_LOOP('',(#1160));
#538=EDGE_LOOP('',(#1161,#1162,#1163,#1164));
#539=EDGE_LOOP('',(#1165));
#540=EDGE_LOOP('',(#1166));
#541=EDGE_LOOP('',(#1167,#1168,#1169,#1170));
#542=EDGE_LOOP('',(#1171));
#543=EDGE_LOOP('',(#1172));
#544=EDGE_LOOP('',(#1173,#1174,#1175,#1176));
#545=EDGE_LOOP('',(#1177,#1178,#1179,#1180));
#546=EDGE_LOOP('',(#1181,#1182,#1183,#1184));
#547=EDGE_LOOP('',(#1185,#1186,#1187,#1188));
#548=EDGE_LOOP('',(#1189));
#549=EDGE_LOOP('',(#1190));
#550=EDGE_LOOP('',(#1191,#1192,#1193,#1194));
#551=EDGE_LOOP('',(#1195,#1196,#1197,#1198));
#552=EDGE_LOOP('',(#1199));
#553=EDGE_LOOP('',(#1200));
#554=EDGE_LOOP('',(#1201,#1202,#1203,#1204));
#555=EDGE_LOOP('',(#1205,#1206,#1207,#1208));
#556=EDGE_LOOP('',(#1209,#1210,#1211,#1212));
#557=EDGE_LOOP('',(#1213));
#558=EDGE_LOOP('',(#1214));
#559=EDGE_LOOP('',(#1215,#1216,#1217,#1218));
#560=EDGE_LOOP('',(#1219,#1220,#1221,#1222));
#561=EDGE_LOOP('',(#1223,#1224,#1225,#1226));
#562=EDGE_LOOP('',(#1227));
#563=EDGE_LOOP('',(#1228));
#564=EDGE_LOOP('',(#1229,#1230,#1231,#1232));
#565=EDGE_LOOP('',(#1233));
#566=EDGE_LOOP('',(#1234));
#567=EDGE_LOOP('',(#1235,#1236,#1237,#1238));
#568=EDGE_LOOP('',(#1239));
#569=EDGE_LOOP('',(#1240));
#570=EDGE_LOOP('',(#1241,#1242,#1243,#1244));
#571=EDGE_LOOP('',(#1245,#1246,#1247,#1248));
#572=EDGE_LOOP('',(#1249,#1250,#1251,#1252));
#573=EDGE_LOOP('',(#1253));
#574=EDGE_LOOP('',(#1254));
#575=EDGE_LOOP('',(#1255,#1256,#1257,#1258));
#576=EDGE_LOOP('',(#1259));
#577=EDGE_LOOP('',(#1260));
#578=EDGE_LOOP('',(#1261,#1262,#1263,#1264));
#579=EDGE_LOOP('',(#1265));
#580=EDGE_LOOP('',(#1266));
#581=EDGE_LOOP('',(#1267,#1268,#1269,#1270));
#582=EDGE_LOOP('',(#1271,#1272,#1273,#1274));
#583=EDGE_LOOP('',(#1275));
#584=EDGE_LOOP('',(#1276));
#585=EDGE_LOOP('',(#1277,#1278,#1279,#1280,#1281,#1282,#1283));
#586=EDGE_LOOP('',(#1284,#1285,#1286,#1287,#1288,#1289,#1290,#1291,#1292));
#587=EDGE_LOOP('',(#1293));
#588=EDGE_LOOP('',(#1294));
#589=EDGE_LOOP('',(#1295));
#590=EDGE_LOOP('',(#1296,#1297,#1298,#1299,#1300));
#591=EDGE_LOOP('',(#1301,#1302,#1303,#1304,#1305));
#592=EDGE_LOOP('',(#1306,#1307,#1308,#1309,#1310));
#593=EDGE_LOOP('',(#1311,#1312,#1313,#1314,#1315));
#594=EDGE_LOOP('',(#1316,#1317,#1318,#1319,#1320));
#595=EDGE_LOOP('',(#1321));
#596=EDGE_LOOP('',(#1322));
#597=EDGE_LOOP('',(#1323));
#598=EDGE_LOOP('',(#1324,#1325,#1326,#1327,#1328));
#599=EDGE_LOOP('',(#1329,#1330,#1331,#1332,#1333));
#600=EDGE_LOOP('',(#1334));
#601=EDGE_LOOP('',(#1335));
#602=EDGE_LOOP('',(#1336));
#603=EDGE_LOOP('',(#1337,#1338,#1339,#1340));
#604=EDGE_LOOP('',(#1341,#1342,#1343,#1344));
#605=EDGE_LOOP('',(#1345));
#606=EDGE_LOOP('',(#1346));
#607=EDGE_LOOP('',(#1347,#1348,#1349,#1350));
#608=EDGE_LOOP('',(#1351,#1352,#1353,#1354));
#609=EDGE_LOOP('',(#1355,#1356,#1357,#1358));
#610=EDGE_LOOP('',(#1359,#1360,#1361,#1362));
#611=EDGE_LOOP('',(#1363,#1364,#1365,#1366));
#612=EDGE_LOOP('',(#1367,#1368,#1369,#1370,#1371));
#613=EDGE_LOOP('',(#1372,#1373,#1374,#1375));
#614=EDGE_LOOP('',(#1376,#1377,#1378,#1379));
#615=EDGE_LOOP('',(#1380,#1381,#1382,#1383,#1384));
#616=EDGE_LOOP('',(#1385,#1386,#1387,#1388));
#617=EDGE_LOOP('',(#1389,#1390,#1391,#1392,#1393));
#618=EDGE_LOOP('',(#1394,#1395,#1396,#1397,#1398,#1399));
#619=EDGE_LOOP('',(#1400,#1401,#1402,#1403,#1404));
#620=EDGE_LOOP('',(#1405,#1406,#1407,#1408,#1409,#1410,#1411,#1412,#1413,
#1414,#1415,#1416));
#621=EDGE_LOOP('',(#1417,#1418,#1419,#1420,#1421,#1422,#1423,#1424,#1425,
#1426,#1427,#1428,#1429,#1430,#1431,#1432));
#622=EDGE_LOOP('',(#1433,#1434,#1435,#1436,#1437,#1438));
#623=EDGE_LOOP('',(#1439,#1440,#1441,#1442,#1443,#1444));
#624=EDGE_LOOP('',(#1445,#1446,#1447,#1448));
#625=EDGE_LOOP('',(#1449,#1450,#1451,#1452));
#626=EDGE_LOOP('',(#1453));
#627=EDGE_LOOP('',(#1454));
#628=EDGE_LOOP('',(#1455,#1456,#1457,#1458));
#629=EDGE_LOOP('',(#1459,#1460,#1461,#1462));
#630=EDGE_LOOP('',(#1463,#1464,#1465,#1466));
#631=EDGE_LOOP('',(#1467,#1468,#1469,#1470));
#632=EDGE_LOOP('',(#1471));
#633=EDGE_LOOP('',(#1472));
#634=EDGE_LOOP('',(#1473,#1474,#1475,#1476));
#635=EDGE_LOOP('',(#1477,#1478,#1479,#1480));
#636=EDGE_LOOP('',(#1481,#1482,#1483,#1484));
#637=EDGE_LOOP('',(#1485));
#638=EDGE_LOOP('',(#1486));
#639=CIRCLE('',#1694,1.78305659323844);
#640=CIRCLE('',#1697,0.600000000000001);
#641=CIRCLE('',#1700,1.19802042656629);
#642=CIRCLE('',#1701,1.19802042656629);
#643=CIRCLE('',#1703,0.898903149093028);
#644=CIRCLE('',#1705,0.898903149093028);
#645=CIRCLE('',#1708,0.898903149093028);
#646=CIRCLE('',#1710,0.898903149093028);
#647=CIRCLE('',#1712,1.80367379624636);
#648=CIRCLE('',#1714,1.80367379624636);
#649=CIRCLE('',#1716,1.9840612380693);
#650=CIRCLE('',#1718,1.9840612380693);
#651=CIRCLE('',#1720,1.49577760563294);
#652=CIRCLE('',#1722,1.49577760563294);
#653=CIRCLE('',#1724,1.24385197034191);
#654=CIRCLE('',#1726,1.24385197034191);
#655=CIRCLE('',#1730,7.3927431617401);
#656=CIRCLE('',#1731,7.3927431617401);
#657=CIRCLE('',#1733,6.8927431617401);
#658=CIRCLE('',#1735,3.57153586442857);
#659=CIRCLE('',#1737,2.54218695620125);
#660=CIRCLE('',#1739,1.93367516017024);
#661=CIRCLE('',#1741,1.93367516017024);
#662=CIRCLE('',#1743,3.68653879426857);
#663=CIRCLE('',#1745,3.68653879426857);
#664=CIRCLE('',#1747,3.10163618786504);
#665=CIRCLE('',#1749,3.10163618786504);
#666=CIRCLE('',#1751,3.37194500132688);
#667=CIRCLE('',#1753,3.37194500132688);
#668=CIRCLE('',#1755,3.62904091081832);
#669=CIRCLE('',#1757,5.34620669590443);
#670=CIRCLE('',#1759,5.84899819199777);
#671=CIRCLE('',#1761,5.84899819199777);
#672=CIRCLE('',#1763,6.35065042485944);
#673=CIRCLE('',#1767,1.49577760563294);
#674=CIRCLE('',#1768,1.15283995859749);
#675=CIRCLE('',#1770,1.15283995859749);
#676=CIRCLE('',#1772,1.99455837231036);
#677=CIRCLE('',#1774,2.3164003912567);
#678=CIRCLE('',#1776,2.3164003912567);
#679=CIRCLE('',#1778,2.02504663208246);
#680=CIRCLE('',#1780,0.94209020647254);
#681=CIRCLE('',#1782,0.94209020647254);
#682=CIRCLE('',#1785,1.02706997925809);
#683=CIRCLE('',#1787,1.02706997925809);
#684=CIRCLE('',#1789,1.49577760563294);
#685=CIRCLE('',#1793,2.3164003912567);
#686=CIRCLE('',#1794,2.06358009076751);
#687=CIRCLE('',#1796,2.3164003912567);
#688=CIRCLE('',#1798,1.99619194538056);
#689=CIRCLE('',#1800,1.99619194538056);
#690=CIRCLE('',#1802,2.3164003912567);
#691=CIRCLE('',#1804,2.3164003912567);
#692=CIRCLE('',#1806,1.93367516017024);
#693=CIRCLE('',#1808,1.16083957311848);
#694=CIRCLE('',#1810,1.16083957311848);
#695=CIRCLE('',#1814,6.22506754791384);
#696=CIRCLE('',#1815,6.22506754791384);
#697=CIRCLE('',#1817,1.);
#698=CIRCLE('',#1819,1.);
#699=CIRCLE('',#1821,1.);
#700=CIRCLE('',#1826,1.);
#701=CIRCLE('',#1829,5.96248981933611);
#702=CIRCLE('',#1830,3.62498032958974);
#703=CIRCLE('',#1833,5.96248981933611);
#704=CIRCLE('',#1835,3.62498032958974);
#705=CIRCLE('',#1837,3.17127539348974);
#706=CIRCLE('',#1839,3.17127539348974);
#707=CIRCLE('',#1846,2.7248783394621);
#708=CIRCLE('',#1847,1.9840612380693);
#709=CIRCLE('',#1853,2.7248783394621);
#710=CIRCLE('',#1854,1.9840612380693);
#711=CIRCLE('',#1855,1.9840612380693);
#712=CIRCLE('',#1856,2.7248783394621);
#713=CIRCLE('',#1859,2.79839874569029);
#714=CIRCLE('',#1860,1.89228053659161);
#715=CIRCLE('',#1861,2.68560675576897);
#716=CIRCLE('',#1862,2.68560675576897);
#717=CIRCLE('',#1864,1.9840612380693);
#718=CIRCLE('',#1865,1.9840612380693);
#719=CIRCLE('',#1866,1.9840612380693);
#720=CIRCLE('',#1868,2.68560675576897);
#721=CIRCLE('',#1870,2.68560675576897);
#722=CIRCLE('',#1874,2.3164003912567);
#723=CIRCLE('',#1876,2.79839874569029);
#724=CIRCLE('',#1878,3.00061238707443);
#725=CIRCLE('',#1880,3.00061238707443);
#726=CIRCLE('',#1882,2.92187821747206);
#727=CIRCLE('',#1884,2.3164003912567);
#728=CIRCLE('',#1888,0.600000000000001);
#729=CIRCLE('',#1889,0.500000000000003);
#730=CIRCLE('',#1891,0.600000000000001);
#731=VERTEX_POINT('',#2410);
#732=VERTEX_POINT('',#2411);
#733=VERTEX_POINT('',#2415);
#734=VERTEX_POINT('',#2416);
#735=VERTEX_POINT('',#2418);
#736=VERTEX_POINT('',#2420);
#737=VERTEX_POINT('',#2422);
#738=VERTEX_POINT('',#2429);
#739=VERTEX_POINT('',#2431);
#740=VERTEX_POINT('',#2449);
#741=VERTEX_POINT('',#2451);
#742=VERTEX_POINT('',#2462);
#743=VERTEX_POINT('',#2491);
#744=VERTEX_POINT('',#2508);
#745=VERTEX_POINT('',#2519);
#746=VERTEX_POINT('',#2529);
#747=VERTEX_POINT('',#2532);
#748=VERTEX_POINT('',#2536);
#749=VERTEX_POINT('',#2540);
#750=VERTEX_POINT('',#2544);
#751=VERTEX_POINT('',#2547);
#752=VERTEX_POINT('',#2552);
#753=VERTEX_POINT('',#2555);
#754=VERTEX_POINT('',#2559);
#755=VERTEX_POINT('',#2562);
#756=VERTEX_POINT('',#2568);
#757=VERTEX_POINT('',#2570);
#758=VERTEX_POINT('',#2574);
#759=VERTEX_POINT('',#2578);
#760=VERTEX_POINT('',#2581);
#761=VERTEX_POINT('',#2585);
#762=VERTEX_POINT('',#2588);
#763=VERTEX_POINT('',#2592);
#764=VERTEX_POINT('',#2595);
#765=VERTEX_POINT('',#2599);
#766=VERTEX_POINT('',#2602);
#767=VERTEX_POINT('',#2606);
#768=VERTEX_POINT('',#2610);
#769=VERTEX_POINT('',#2614);
#770=VERTEX_POINT('',#2618);
#771=VERTEX_POINT('',#2621);
#772=VERTEX_POINT('',#2625);
#773=VERTEX_POINT('',#2629);
#774=VERTEX_POINT('',#2635);
#775=VERTEX_POINT('',#2637);
#776=VERTEX_POINT('',#2641);
#777=VERTEX_POINT('',#2645);
#778=VERTEX_POINT('',#2648);
#779=VERTEX_POINT('',#2652);
#780=VERTEX_POINT('',#2656);
#781=VERTEX_POINT('',#2660);
#782=VERTEX_POINT('',#2663);
#783=VERTEX_POINT('',#2668);
#784=VERTEX_POINT('',#2671);
#785=VERTEX_POINT('',#2675);
#786=VERTEX_POINT('',#2681);
#787=VERTEX_POINT('',#2683);
#788=VERTEX_POINT('',#2687);
#789=VERTEX_POINT('',#2691);
#790=VERTEX_POINT('',#2694);
#791=VERTEX_POINT('',#2698);
#792=VERTEX_POINT('',#2701);
#793=VERTEX_POINT('',#2705);
#794=VERTEX_POINT('',#2708);
#795=VERTEX_POINT('',#2712);
#796=VERTEX_POINT('',#2825);
#797=VERTEX_POINT('',#2826);
#798=VERTEX_POINT('',#2828);
#799=VERTEX_POINT('',#2909);
#800=VERTEX_POINT('',#2928);
#801=VERTEX_POINT('',#2976);
#802=VERTEX_POINT('',#2979);
#803=VERTEX_POINT('',#2982);
#804=VERTEX_POINT('',#3149);
#805=VERTEX_POINT('',#3307);
#806=VERTEX_POINT('',#3466);
#807=VERTEX_POINT('',#3585);
#808=VERTEX_POINT('',#3587);
#809=VERTEX_POINT('',#3825);
#810=VERTEX_POINT('',#3936);
#811=VERTEX_POINT('',#3938);
#812=VERTEX_POINT('',#4124);
#813=VERTEX_POINT('',#4250);
#814=VERTEX_POINT('',#4252);
#815=VERTEX_POINT('',#4326);
#816=VERTEX_POINT('',#4331);
#817=VERTEX_POINT('',#4333);
#818=VERTEX_POINT('',#4338);
#819=VERTEX_POINT('',#4342);
#820=VERTEX_POINT('',#4345);
#821=VERTEX_POINT('',#4349);
#822=VERTEX_POINT('',#4356);
#823=VERTEX_POINT('',#4357);
#824=VERTEX_POINT('',#4359);
#825=VERTEX_POINT('',#4361);
#826=VERTEX_POINT('',#4365);
#827=VERTEX_POINT('',#4366);
#828=VERTEX_POINT('',#4368);
#829=VERTEX_POINT('',#4370);
#830=VERTEX_POINT('',#4374);
#831=VERTEX_POINT('',#4381);
#832=VERTEX_POINT('',#4392);
#833=VERTEX_POINT('',#4408);
#834=VERTEX_POINT('',#4410);
#835=VERTEX_POINT('',#4414);
#836=VERTEX_POINT('',#4415);
#837=VERTEX_POINT('',#4417);
#838=VERTEX_POINT('',#4419);
#839=VERTEX_POINT('',#4423);
#840=VERTEX_POINT('',#4454);
#841=VERTEX_POINT('',#4455);
#842=VERTEX_POINT('',#4457);
#843=VERTEX_POINT('',#4459);
#844=VERTEX_POINT('',#4463);
#845=VERTEX_POINT('',#4464);
#846=VERTEX_POINT('',#4481);
#847=VERTEX_POINT('',#4494);
#848=VERTEX_POINT('',#4496);
#849=VERTEX_POINT('',#4498);
#850=VERTEX_POINT('',#4500);
#851=VERTEX_POINT('',#4504);
#852=VERTEX_POINT('',#4532);
#853=VERTEX_POINT('',#4538);
#854=VERTEX_POINT('',#4550);
#855=VERTEX_POINT('',#4553);
#856=VERTEX_POINT('',#4557);
#857=VERTEX_POINT('',#4561);
#858=VERTEX_POINT('',#4565);
#859=VERTEX_POINT('',#4569);
#860=VERTEX_POINT('',#4575);
#861=VERTEX_POINT('',#4577);
#862=VERTEX_POINT('',#4581);
#863=EDGE_CURVE('',#731,#732,#639,.T.);
#864=EDGE_CURVE('',#733,#734,#165,.T.);
#865=EDGE_CURVE('',#733,#735,#640,.T.);
#866=EDGE_CURVE('',#736,#735,#166,.T.);
#867=EDGE_CURVE('',#737,#736,#132,.T.);
#868=EDGE_CURVE('',#738,#737,#167,.T.);
#869=EDGE_CURVE('',#739,#738,#133,.T.);
#870=EDGE_CURVE('',#739,#740,#168,.T.);
#871=EDGE_CURVE('',#741,#740,#134,.T.);
#872=EDGE_CURVE('',#742,#741,#135,.T.);
#873=EDGE_CURVE('',#740,#742,#136,.T.);
#874=EDGE_CURVE('',#743,#739,#137,.T.);
#875=EDGE_CURVE('',#744,#743,#169,.T.);
#876=EDGE_CURVE('',#734,#744,#138,.T.);
#877=EDGE_CURVE('',#735,#733,#170,.T.);
#878=EDGE_CURVE('',#745,#745,#641,.T.);
#879=EDGE_CURVE('',#745,#739,#171,.T.);
#880=EDGE_CURVE('',#738,#743,#642,.T.);
#881=EDGE_CURVE('',#736,#734,#643,.T.);
#882=EDGE_CURVE('',#737,#744,#644,.T.);
#883=EDGE_CURVE('',#746,#746,#645,.T.);
#884=EDGE_CURVE('',#747,#747,#646,.T.);
#885=EDGE_CURVE('',#747,#746,#172,.T.);
#886=EDGE_CURVE('',#747,#748,#173,.T.);
#887=EDGE_CURVE('',#748,#748,#647,.T.);
#888=EDGE_CURVE('',#749,#749,#648,.T.);
#889=EDGE_CURVE('',#749,#748,#174,.T.);
#890=EDGE_CURVE('',#750,#750,#649,.T.);
#891=EDGE_CURVE('',#751,#751,#650,.T.);
#892=EDGE_CURVE('',#751,#742,#175,.T.);
#893=EDGE_CURVE('',#740,#750,#176,.T.);
#894=EDGE_CURVE('',#752,#752,#651,.T.);
#895=EDGE_CURVE('',#753,#753,#652,.T.);
#896=EDGE_CURVE('',#753,#752,#177,.T.);
#897=EDGE_CURVE('',#754,#754,#653,.T.);
#898=EDGE_CURVE('',#755,#755,#654,.T.);
#899=EDGE_CURVE('',#755,#754,#178,.T.);
#900=EDGE_CURVE('',#756,#756,#655,.T.);
#901=EDGE_CURVE('',#756,#757,#179,.T.);
#902=EDGE_CURVE('',#757,#757,#656,.T.);
#903=EDGE_CURVE('',#756,#758,#180,.T.);
#904=EDGE_CURVE('',#758,#758,#657,.T.);
#905=EDGE_CURVE('',#759,#759,#658,.T.);
#906=EDGE_CURVE('',#760,#760,#659,.T.);
#907=EDGE_CURVE('',#760,#759,#181,.T.);
#908=EDGE_CURVE('',#761,#761,#660,.T.);
#909=EDGE_CURVE('',#762,#762,#661,.T.);
#910=EDGE_CURVE('',#762,#761,#182,.T.);
#911=EDGE_CURVE('',#763,#763,#662,.T.);
#912=EDGE_CURVE('',#764,#764,#663,.T.);
#913=EDGE_CURVE('',#764,#763,#183,.T.);
#914=EDGE_CURVE('',#765,#765,#664,.T.);
#915=EDGE_CURVE('',#766,#766,#665,.T.);
#916=EDGE_CURVE('',#766,#765,#184,.T.);
#917=EDGE_CURVE('',#766,#767,#185,.T.);
#918=EDGE_CURVE('',#767,#767,#666,.T.);
#919=EDGE_CURVE('',#768,#768,#667,.T.);
#920=EDGE_CURVE('',#768,#767,#186,.T.);
#921=EDGE_CURVE('',#768,#769,#187,.T.);
#922=EDGE_CURVE('',#769,#769,#668,.T.);
#923=EDGE_CURVE('',#770,#770,#669,.T.);
#924=EDGE_CURVE('',#771,#771,#670,.T.);
#925=EDGE_CURVE('',#771,#770,#188,.T.);
#926=EDGE_CURVE('',#772,#772,#671,.T.);
#927=EDGE_CURVE('',#772,#771,#189,.T.);
#928=EDGE_CURVE('',#773,#773,#672,.T.);
#929=EDGE_CURVE('',#757,#773,#190,.T.);
#930=EDGE_CURVE('',#774,#774,#673,.T.);
#931=EDGE_CURVE('',#774,#775,#191,.T.);
#932=EDGE_CURVE('',#775,#775,#674,.T.);
#933=EDGE_CURVE('',#776,#776,#675,.T.);
#934=EDGE_CURVE('',#776,#775,#192,.T.);
#935=EDGE_CURVE('',#777,#777,#676,.T.);
#936=EDGE_CURVE('',#778,#778,#677,.T.);
#937=EDGE_CURVE('',#778,#777,#193,.T.);
#938=EDGE_CURVE('',#779,#779,#678,.T.);
#939=EDGE_CURVE('',#779,#778,#194,.T.);
#940=EDGE_CURVE('',#779,#780,#195,.T.);
#941=EDGE_CURVE('',#780,#780,#679,.T.);
#942=EDGE_CURVE('',#781,#781,#680,.T.);
#943=EDGE_CURVE('',#782,#782,#681,.T.);
#944=EDGE_CURVE('',#782,#781,#196,.T.);
#945=EDGE_CURVE('',#783,#783,#682,.T.);
#946=EDGE_CURVE('',#784,#784,#683,.T.);
#947=EDGE_CURVE('',#784,#783,#197,.T.);
#948=EDGE_CURVE('',#785,#785,#684,.T.);
#949=EDGE_CURVE('',#774,#785,#198,.T.);
#950=EDGE_CURVE('',#786,#786,#685,.T.);
#951=EDGE_CURVE('',#786,#787,#199,.T.);
#952=EDGE_CURVE('',#787,#787,#686,.T.);
#953=EDGE_CURVE('',#788,#788,#687,.T.);
#954=EDGE_CURVE('',#788,#786,#200,.T.);
#955=EDGE_CURVE('',#789,#789,#688,.T.);
#956=EDGE_CURVE('',#790,#790,#689,.T.);
#957=EDGE_CURVE('',#790,#789,#201,.T.);
#958=EDGE_CURVE('',#791,#791,#690,.T.);
#959=EDGE_CURVE('',#792,#792,#691,.T.);
#960=EDGE_CURVE('',#792,#791,#202,.T.);
#961=EDGE_CURVE('',#793,#793,#692,.T.);
#962=EDGE_CURVE('',#794,#794,#693,.T.);
#963=EDGE_CURVE('',#794,#793,#203,.T.);
#964=EDGE_CURVE('',#795,#795,#694,.T.);
#965=EDGE_CURVE('',#795,#794,#204,.T.);
#966=EDGE_CURVE('',#796,#797,#205,.T.);
#967=EDGE_CURVE('',#797,#798,#139,.T.);
#968=EDGE_CURVE('',#798,#797,#140,.T.);
#969=EDGE_CURVE('',#796,#799,#141,.T.);
#970=EDGE_CURVE('',#799,#800,#142,.T.);
#971=EDGE_CURVE('',#800,#796,#143,.T.);
#972=EDGE_CURVE('',#801,#801,#695,.T.);
#973=EDGE_CURVE('',#801,#799,#206,.T.);
#974=EDGE_CURVE('',#800,#802,#207,.T.);
#975=EDGE_CURVE('',#802,#802,#696,.T.);
#976=EDGE_CURVE('',#803,#803,#144,.T.);
#977=EDGE_CURVE('',#804,#804,#145,.T.);
#978=EDGE_CURVE('',#805,#805,#146,.T.);
#979=EDGE_CURVE('',#806,#806,#697,.T.);
#980=EDGE_CURVE('',#806,#798,#208,.T.);
#981=EDGE_CURVE('',#803,#807,#209,.T.);
#982=EDGE_CURVE('',#807,#808,#147,.T.);
#983=EDGE_CURVE('',#808,#807,#148,.T.);
#984=EDGE_CURVE('',#809,#809,#698,.T.);
#985=EDGE_CURVE('',#809,#808,#210,.T.);
#986=EDGE_CURVE('',#805,#810,#211,.T.);
#987=EDGE_CURVE('',#810,#811,#149,.T.);
#988=EDGE_CURVE('',#811,#810,#150,.T.);
#989=EDGE_CURVE('',#812,#812,#699,.T.);
#990=EDGE_CURVE('',#812,#811,#212,.T.);
#991=EDGE_CURVE('',#804,#813,#213,.T.);
#992=EDGE_CURVE('',#813,#814,#151,.T.);
#993=EDGE_CURVE('',#814,#813,#152,.T.);
#994=EDGE_CURVE('',#815,#815,#700,.T.);
#995=EDGE_CURVE('',#815,#814,#214,.T.);
#996=EDGE_CURVE('',#816,#816,#701,.T.);
#997=EDGE_CURVE('',#817,#817,#702,.T.);
#998=EDGE_CURVE('',#802,#816,#215,.T.);
#999=EDGE_CURVE('',#801,#818,#216,.T.);
#1000=EDGE_CURVE('',#818,#818,#703,.T.);
#1001=EDGE_CURVE('',#819,#819,#704,.T.);
#1002=EDGE_CURVE('',#820,#820,#705,.T.);
#1003=EDGE_CURVE('',#820,#819,#217,.T.);
#1004=EDGE_CURVE('',#821,#821,#706,.T.);
#1005=EDGE_CURVE('',#821,#820,#218,.T.);
#1006=EDGE_CURVE('',#821,#817,#219,.T.);
#1007=EDGE_CURVE('',#822,#823,#220,.T.);
#1008=EDGE_CURVE('',#824,#822,#221,.T.);
#1009=EDGE_CURVE('',#825,#824,#222,.T.);
#1010=EDGE_CURVE('',#825,#823,#223,.T.);
#1011=EDGE_CURVE('',#826,#827,#224,.T.);
#1012=EDGE_CURVE('',#826,#828,#225,.T.);
#1013=EDGE_CURVE('',#829,#828,#226,.T.);
#1014=EDGE_CURVE('',#827,#829,#227,.T.);
#1015=EDGE_CURVE('',#823,#830,#153,.T.);
#1016=EDGE_CURVE('',#831,#825,#154,.T.);
#1017=EDGE_CURVE('',#832,#831,#228,.T.);
#1018=EDGE_CURVE('',#830,#832,#155,.T.);
#1019=EDGE_CURVE('',#832,#833,#707,.T.);
#1020=EDGE_CURVE('',#834,#831,#708,.T.);
#1021=EDGE_CURVE('',#833,#834,#229,.T.);
#1022=EDGE_CURVE('',#835,#836,#230,.T.);
#1023=EDGE_CURVE('',#835,#837,#231,.T.);
#1024=EDGE_CURVE('',#838,#837,#232,.T.);
#1025=EDGE_CURVE('',#836,#838,#233,.T.);
#1026=EDGE_CURVE('',#833,#839,#156,.T.);
#1027=EDGE_CURVE('',#837,#834,#157,.T.);
#1028=EDGE_CURVE('',#839,#835,#158,.T.);
#1029=EDGE_CURVE('',#840,#841,#234,.T.);
#1030=EDGE_CURVE('',#842,#840,#235,.T.);
#1031=EDGE_CURVE('',#843,#842,#236,.T.);
#1032=EDGE_CURVE('',#843,#841,#237,.T.);
#1033=EDGE_CURVE('',#844,#845,#159,.T.);
#1034=EDGE_CURVE('',#841,#844,#160,.T.);
#1035=EDGE_CURVE('',#846,#843,#161,.T.);
#1036=EDGE_CURVE('',#846,#845,#238,.T.);
#1037=EDGE_CURVE('',#845,#847,#709,.T.);
#1038=EDGE_CURVE('',#848,#846,#710,.T.);
#1039=EDGE_CURVE('',#849,#848,#711,.T.);
#1040=EDGE_CURVE('',#849,#850,#239,.T.);
#1041=EDGE_CURVE('',#847,#850,#712,.T.);
#1042=EDGE_CURVE('',#851,#826,#162,.T.);
#1043=EDGE_CURVE('',#850,#851,#163,.T.);
#1044=EDGE_CURVE('',#828,#849,#164,.T.);
#1045=EDGE_CURVE('',#852,#852,#713,.T.);
#1046=EDGE_CURVE('',#852,#847,#714,.T.);
#1047=EDGE_CURVE('',#851,#830,#715,.T.);
#1048=EDGE_CURVE('',#839,#844,#716,.T.);
#1049=EDGE_CURVE('',#848,#853,#240,.T.);
#1050=EDGE_CURVE('',#853,#853,#717,.T.);
#1051=EDGE_CURVE('',#838,#842,#718,.T.);
#1052=EDGE_CURVE('',#829,#824,#719,.T.);
#1053=EDGE_CURVE('',#836,#840,#720,.T.);
#1054=EDGE_CURVE('',#827,#822,#721,.T.);
#1055=EDGE_CURVE('',#854,#854,#722,.T.);
#1056=EDGE_CURVE('',#855,#855,#723,.T.);
#1057=EDGE_CURVE('',#855,#852,#241,.T.);
#1058=EDGE_CURVE('',#856,#856,#724,.T.);
#1059=EDGE_CURVE('',#856,#855,#242,.T.);
#1060=EDGE_CURVE('',#857,#857,#725,.T.);
#1061=EDGE_CURVE('',#857,#856,#243,.T.);
#1062=EDGE_CURVE('',#857,#858,#244,.T.);
#1063=EDGE_CURVE('',#858,#858,#726,.T.);
#1064=EDGE_CURVE('',#859,#859,#727,.T.);
#1065=EDGE_CURVE('',#854,#859,#245,.T.);
#1066=EDGE_CURVE('',#860,#860,#728,.T.);
#1067=EDGE_CURVE('',#860,#861,#246,.T.);
#1068=EDGE_CURVE('',#861,#861,#729,.T.);
#1069=EDGE_CURVE('',#860,#862,#247,.T.);
#1070=EDGE_CURVE('',#862,#862,#730,.T.);
#1071=ORIENTED_EDGE('',*,*,#863,.T.);
#1072=ORIENTED_EDGE('',*,*,#863,.F.);
#1073=ORIENTED_EDGE('',*,*,#864,.F.);
#1074=ORIENTED_EDGE('',*,*,#865,.T.);
#1075=ORIENTED_EDGE('',*,*,#866,.F.);
#1076=ORIENTED_EDGE('',*,*,#867,.F.);
#1077=ORIENTED_EDGE('',*,*,#868,.F.);
#1078=ORIENTED_EDGE('',*,*,#869,.F.);
#1079=ORIENTED_EDGE('',*,*,#870,.T.);
#1080=ORIENTED_EDGE('',*,*,#871,.F.);
#1081=ORIENTED_EDGE('',*,*,#872,.F.);
#1082=ORIENTED_EDGE('',*,*,#873,.F.);
#1083=ORIENTED_EDGE('',*,*,#870,.F.);
#1084=ORIENTED_EDGE('',*,*,#874,.F.);
#1085=ORIENTED_EDGE('',*,*,#875,.F.);
#1086=ORIENTED_EDGE('',*,*,#876,.F.);
#1087=ORIENTED_EDGE('',*,*,#877,.F.);
#1088=ORIENTED_EDGE('',*,*,#865,.F.);
#1089=ORIENTED_EDGE('',*,*,#878,.F.);
#1090=ORIENTED_EDGE('',*,*,#879,.T.);
#1091=ORIENTED_EDGE('',*,*,#869,.T.);
#1092=ORIENTED_EDGE('',*,*,#880,.T.);
#1093=ORIENTED_EDGE('',*,*,#874,.T.);
#1094=ORIENTED_EDGE('',*,*,#879,.F.);
#1095=ORIENTED_EDGE('',*,*,#864,.T.);
#1096=ORIENTED_EDGE('',*,*,#881,.F.);
#1097=ORIENTED_EDGE('',*,*,#866,.T.);
#1098=ORIENTED_EDGE('',*,*,#877,.T.);
#1099=ORIENTED_EDGE('',*,*,#876,.T.);
#1100=ORIENTED_EDGE('',*,*,#882,.F.);
#1101=ORIENTED_EDGE('',*,*,#867,.T.);
#1102=ORIENTED_EDGE('',*,*,#881,.T.);
#1103=ORIENTED_EDGE('',*,*,#875,.T.);
#1104=ORIENTED_EDGE('',*,*,#880,.F.);
#1105=ORIENTED_EDGE('',*,*,#868,.T.);
#1106=ORIENTED_EDGE('',*,*,#882,.T.);
#1107=ORIENTED_EDGE('',*,*,#878,.T.);
#1108=ORIENTED_EDGE('',*,*,#883,.F.);
#1109=ORIENTED_EDGE('',*,*,#884,.F.);
#1110=ORIENTED_EDGE('',*,*,#885,.T.);
#1111=ORIENTED_EDGE('',*,*,#883,.T.);
#1112=ORIENTED_EDGE('',*,*,#885,.F.);
#1113=ORIENTED_EDGE('',*,*,#884,.T.);
#1114=ORIENTED_EDGE('',*,*,#886,.T.);
#1115=ORIENTED_EDGE('',*,*,#887,.F.);
#1116=ORIENTED_EDGE('',*,*,#886,.F.);
#1117=ORIENTED_EDGE('',*,*,#888,.F.);
#1118=ORIENTED_EDGE('',*,*,#889,.T.);
#1119=ORIENTED_EDGE('',*,*,#887,.T.);
#1120=ORIENTED_EDGE('',*,*,#889,.F.);
#1121=ORIENTED_EDGE('',*,*,#890,.F.);
#1122=ORIENTED_EDGE('',*,*,#888,.T.);
#1123=ORIENTED_EDGE('',*,*,#891,.F.);
#1124=ORIENTED_EDGE('',*,*,#892,.T.);
#1125=ORIENTED_EDGE('',*,*,#872,.T.);
#1126=ORIENTED_EDGE('',*,*,#871,.T.);
#1127=ORIENTED_EDGE('',*,*,#893,.T.);
#1128=ORIENTED_EDGE('',*,*,#890,.T.);
#1129=ORIENTED_EDGE('',*,*,#893,.F.);
#1130=ORIENTED_EDGE('',*,*,#873,.T.);
#1131=ORIENTED_EDGE('',*,*,#892,.F.);
#1132=ORIENTED_EDGE('',*,*,#891,.T.);
#1133=ORIENTED_EDGE('',*,*,#894,.F.);
#1134=ORIENTED_EDGE('',*,*,#895,.F.);
#1135=ORIENTED_EDGE('',*,*,#896,.T.);
#1136=ORIENTED_EDGE('',*,*,#894,.T.);
#1137=ORIENTED_EDGE('',*,*,#896,.F.);
#1138=ORIENTED_EDGE('',*,*,#895,.T.);
#1139=ORIENTED_EDGE('',*,*,#897,.F.);
#1140=ORIENTED_EDGE('',*,*,#898,.F.);
#1141=ORIENTED_EDGE('',*,*,#899,.T.);
#1142=ORIENTED_EDGE('',*,*,#897,.T.);
#1143=ORIENTED_EDGE('',*,*,#899,.F.);
#1144=ORIENTED_EDGE('',*,*,#898,.T.);
#1145=ORIENTED_EDGE('',*,*,#900,.F.);
#1146=ORIENTED_EDGE('',*,*,#901,.T.);
#1147=ORIENTED_EDGE('',*,*,#902,.T.);
#1148=ORIENTED_EDGE('',*,*,#901,.F.);
#1149=ORIENTED_EDGE('',*,*,#900,.T.);
#1150=ORIENTED_EDGE('',*,*,#903,.T.);
#1151=ORIENTED_EDGE('',*,*,#904,.F.);
#1152=ORIENTED_EDGE('',*,*,#903,.F.);
#1153=ORIENTED_EDGE('',*,*,#904,.T.);
#1154=ORIENTED_EDGE('',*,*,#905,.F.);
#1155=ORIENTED_EDGE('',*,*,#906,.F.);
#1156=ORIENTED_EDGE('',*,*,#907,.T.);
#1157=ORIENTED_EDGE('',*,*,#905,.T.);
#1158=ORIENTED_EDGE('',*,*,#907,.F.);
#1159=ORIENTED_EDGE('',*,*,#906,.T.);
#1160=ORIENTED_EDGE('',*,*,#908,.F.);
#1161=ORIENTED_EDGE('',*,*,#909,.F.);
#1162=ORIENTED_EDGE('',*,*,#910,.T.);
#1163=ORIENTED_EDGE('',*,*,#908,.T.);
#1164=ORIENTED_EDGE('',*,*,#910,.F.);
#1165=ORIENTED_EDGE('',*,*,#911,.F.);
#1166=ORIENTED_EDGE('',*,*,#909,.T.);
#1167=ORIENTED_EDGE('',*,*,#912,.F.);
#1168=ORIENTED_EDGE('',*,*,#913,.T.);
#1169=ORIENTED_EDGE('',*,*,#911,.T.);
#1170=ORIENTED_EDGE('',*,*,#913,.F.);
#1171=ORIENTED_EDGE('',*,*,#912,.T.);
#1172=ORIENTED_EDGE('',*,*,#914,.F.);
#1173=ORIENTED_EDGE('',*,*,#915,.F.);
#1174=ORIENTED_EDGE('',*,*,#916,.T.);
#1175=ORIENTED_EDGE('',*,*,#914,.T.);
#1176=ORIENTED_EDGE('',*,*,#916,.F.);
#1177=ORIENTED_EDGE('',*,*,#915,.T.);
#1178=ORIENTED_EDGE('',*,*,#917,.T.);
#1179=ORIENTED_EDGE('',*,*,#918,.F.);
#1180=ORIENTED_EDGE('',*,*,#917,.F.);
#1181=ORIENTED_EDGE('',*,*,#919,.F.);
#1182=ORIENTED_EDGE('',*,*,#920,.T.);
#1183=ORIENTED_EDGE('',*,*,#918,.T.);
#1184=ORIENTED_EDGE('',*,*,#920,.F.);
#1185=ORIENTED_EDGE('',*,*,#919,.T.);
#1186=ORIENTED_EDGE('',*,*,#921,.T.);
#1187=ORIENTED_EDGE('',*,*,#922,.F.);
#1188=ORIENTED_EDGE('',*,*,#921,.F.);
#1189=ORIENTED_EDGE('',*,*,#923,.F.);
#1190=ORIENTED_EDGE('',*,*,#922,.T.);
#1191=ORIENTED_EDGE('',*,*,#924,.F.);
#1192=ORIENTED_EDGE('',*,*,#925,.T.);
#1193=ORIENTED_EDGE('',*,*,#923,.T.);
#1194=ORIENTED_EDGE('',*,*,#925,.F.);
#1195=ORIENTED_EDGE('',*,*,#926,.F.);
#1196=ORIENTED_EDGE('',*,*,#927,.T.);
#1197=ORIENTED_EDGE('',*,*,#924,.T.);
#1198=ORIENTED_EDGE('',*,*,#927,.F.);
#1199=ORIENTED_EDGE('',*,*,#928,.F.);
#1200=ORIENTED_EDGE('',*,*,#926,.T.);
#1201=ORIENTED_EDGE('',*,*,#902,.F.);
#1202=ORIENTED_EDGE('',*,*,#929,.T.);
#1203=ORIENTED_EDGE('',*,*,#928,.T.);
#1204=ORIENTED_EDGE('',*,*,#929,.F.);
#1205=ORIENTED_EDGE('',*,*,#930,.T.);
#1206=ORIENTED_EDGE('',*,*,#931,.T.);
#1207=ORIENTED_EDGE('',*,*,#932,.F.);
#1208=ORIENTED_EDGE('',*,*,#931,.F.);
#1209=ORIENTED_EDGE('',*,*,#933,.F.);
#1210=ORIENTED_EDGE('',*,*,#934,.T.);
#1211=ORIENTED_EDGE('',*,*,#932,.T.);
#1212=ORIENTED_EDGE('',*,*,#934,.F.);
#1213=ORIENTED_EDGE('',*,*,#935,.F.);
#1214=ORIENTED_EDGE('',*,*,#933,.T.);
#1215=ORIENTED_EDGE('',*,*,#936,.F.);
#1216=ORIENTED_EDGE('',*,*,#937,.T.);
#1217=ORIENTED_EDGE('',*,*,#935,.T.);
#1218=ORIENTED_EDGE('',*,*,#937,.F.);
#1219=ORIENTED_EDGE('',*,*,#938,.F.);
#1220=ORIENTED_EDGE('',*,*,#939,.T.);
#1221=ORIENTED_EDGE('',*,*,#936,.T.);
#1222=ORIENTED_EDGE('',*,*,#939,.F.);
#1223=ORIENTED_EDGE('',*,*,#938,.T.);
#1224=ORIENTED_EDGE('',*,*,#940,.T.);
#1225=ORIENTED_EDGE('',*,*,#941,.F.);
#1226=ORIENTED_EDGE('',*,*,#940,.F.);
#1227=ORIENTED_EDGE('',*,*,#941,.T.);
#1228=ORIENTED_EDGE('',*,*,#942,.F.);
#1229=ORIENTED_EDGE('',*,*,#943,.F.);
#1230=ORIENTED_EDGE('',*,*,#944,.T.);
#1231=ORIENTED_EDGE('',*,*,#942,.T.);
#1232=ORIENTED_EDGE('',*,*,#944,.F.);
#1233=ORIENTED_EDGE('',*,*,#943,.T.);
#1234=ORIENTED_EDGE('',*,*,#945,.F.);
#1235=ORIENTED_EDGE('',*,*,#946,.F.);
#1236=ORIENTED_EDGE('',*,*,#947,.T.);
#1237=ORIENTED_EDGE('',*,*,#945,.T.);
#1238=ORIENTED_EDGE('',*,*,#947,.F.);
#1239=ORIENTED_EDGE('',*,*,#948,.F.);
#1240=ORIENTED_EDGE('',*,*,#946,.T.);
#1241=ORIENTED_EDGE('',*,*,#930,.F.);
#1242=ORIENTED_EDGE('',*,*,#949,.T.);
#1243=ORIENTED_EDGE('',*,*,#948,.T.);
#1244=ORIENTED_EDGE('',*,*,#949,.F.);
#1245=ORIENTED_EDGE('',*,*,#950,.F.);
#1246=ORIENTED_EDGE('',*,*,#951,.T.);
#1247=ORIENTED_EDGE('',*,*,#952,.T.);
#1248=ORIENTED_EDGE('',*,*,#951,.F.);
#1249=ORIENTED_EDGE('',*,*,#953,.F.);
#1250=ORIENTED_EDGE('',*,*,#954,.T.);
#1251=ORIENTED_EDGE('',*,*,#950,.T.);
#1252=ORIENTED_EDGE('',*,*,#954,.F.);
#1253=ORIENTED_EDGE('',*,*,#953,.T.);
#1254=ORIENTED_EDGE('',*,*,#955,.F.);
#1255=ORIENTED_EDGE('',*,*,#956,.F.);
#1256=ORIENTED_EDGE('',*,*,#957,.T.);
#1257=ORIENTED_EDGE('',*,*,#955,.T.);
#1258=ORIENTED_EDGE('',*,*,#957,.F.);
#1259=ORIENTED_EDGE('',*,*,#958,.F.);
#1260=ORIENTED_EDGE('',*,*,#956,.T.);
#1261=ORIENTED_EDGE('',*,*,#959,.F.);
#1262=ORIENTED_EDGE('',*,*,#960,.T.);
#1263=ORIENTED_EDGE('',*,*,#958,.T.);
#1264=ORIENTED_EDGE('',*,*,#960,.F.);
#1265=ORIENTED_EDGE('',*,*,#959,.T.);
#1266=ORIENTED_EDGE('',*,*,#961,.F.);
#1267=ORIENTED_EDGE('',*,*,#962,.F.);
#1268=ORIENTED_EDGE('',*,*,#963,.T.);
#1269=ORIENTED_EDGE('',*,*,#961,.T.);
#1270=ORIENTED_EDGE('',*,*,#963,.F.);
#1271=ORIENTED_EDGE('',*,*,#964,.F.);
#1272=ORIENTED_EDGE('',*,*,#965,.T.);
#1273=ORIENTED_EDGE('',*,*,#962,.T.);
#1274=ORIENTED_EDGE('',*,*,#965,.F.);
#1275=ORIENTED_EDGE('',*,*,#952,.F.);
#1276=ORIENTED_EDGE('',*,*,#964,.T.);
#1277=ORIENTED_EDGE('',*,*,#966,.T.);
#1278=ORIENTED_EDGE('',*,*,#967,.T.);
#1279=ORIENTED_EDGE('',*,*,#968,.T.);
#1280=ORIENTED_EDGE('',*,*,#966,.F.);
#1281=ORIENTED_EDGE('',*,*,#969,.T.);
#1282=ORIENTED_EDGE('',*,*,#970,.T.);
#1283=ORIENTED_EDGE('',*,*,#971,.T.);
#1284=ORIENTED_EDGE('',*,*,#972,.F.);
#1285=ORIENTED_EDGE('',*,*,#973,.T.);
#1286=ORIENTED_EDGE('',*,*,#969,.F.);
#1287=ORIENTED_EDGE('',*,*,#971,.F.);
#1288=ORIENTED_EDGE('',*,*,#974,.T.);
#1289=ORIENTED_EDGE('',*,*,#975,.T.);
#1290=ORIENTED_EDGE('',*,*,#974,.F.);
#1291=ORIENTED_EDGE('',*,*,#970,.F.);
#1292=ORIENTED_EDGE('',*,*,#973,.F.);
#1293=ORIENTED_EDGE('',*,*,#976,.F.);
#1294=ORIENTED_EDGE('',*,*,#977,.F.);
#1295=ORIENTED_EDGE('',*,*,#978,.F.);
#1296=ORIENTED_EDGE('',*,*,#979,.F.);
#1297=ORIENTED_EDGE('',*,*,#980,.T.);
#1298=ORIENTED_EDGE('',*,*,#967,.F.);
#1299=ORIENTED_EDGE('',*,*,#968,.F.);
#1300=ORIENTED_EDGE('',*,*,#980,.F.);
#1301=ORIENTED_EDGE('',*,*,#981,.T.);
#1302=ORIENTED_EDGE('',*,*,#982,.T.);
#1303=ORIENTED_EDGE('',*,*,#983,.T.);
#1304=ORIENTED_EDGE('',*,*,#981,.F.);
#1305=ORIENTED_EDGE('',*,*,#976,.T.);
#1306=ORIENTED_EDGE('',*,*,#984,.F.);
#1307=ORIENTED_EDGE('',*,*,#985,.T.);
#1308=ORIENTED_EDGE('',*,*,#982,.F.);
#1309=ORIENTED_EDGE('',*,*,#983,.F.);
#1310=ORIENTED_EDGE('',*,*,#985,.F.);
#1311=ORIENTED_EDGE('',*,*,#986,.T.);
#1312=ORIENTED_EDGE('',*,*,#987,.T.);
#1313=ORIENTED_EDGE('',*,*,#988,.T.);
#1314=ORIENTED_EDGE('',*,*,#986,.F.);
#1315=ORIENTED_EDGE('',*,*,#978,.T.);
#1316=ORIENTED_EDGE('',*,*,#989,.F.);
#1317=ORIENTED_EDGE('',*,*,#990,.T.);
#1318=ORIENTED_EDGE('',*,*,#987,.F.);
#1319=ORIENTED_EDGE('',*,*,#988,.F.);
#1320=ORIENTED_EDGE('',*,*,#990,.F.);
#1321=ORIENTED_EDGE('',*,*,#979,.T.);
#1322=ORIENTED_EDGE('',*,*,#984,.T.);
#1323=ORIENTED_EDGE('',*,*,#989,.T.);
#1324=ORIENTED_EDGE('',*,*,#991,.T.);
#1325=ORIENTED_EDGE('',*,*,#992,.T.);
#1326=ORIENTED_EDGE('',*,*,#993,.T.);
#1327=ORIENTED_EDGE('',*,*,#991,.F.);
#1328=ORIENTED_EDGE('',*,*,#977,.T.);
#1329=ORIENTED_EDGE('',*,*,#994,.F.);
#1330=ORIENTED_EDGE('',*,*,#995,.T.);
#1331=ORIENTED_EDGE('',*,*,#992,.F.);
#1332=ORIENTED_EDGE('',*,*,#993,.F.);
#1333=ORIENTED_EDGE('',*,*,#995,.F.);
#1334=ORIENTED_EDGE('',*,*,#994,.T.);
#1335=ORIENTED_EDGE('',*,*,#996,.F.);
#1336=ORIENTED_EDGE('',*,*,#997,.T.);
#1337=ORIENTED_EDGE('',*,*,#975,.F.);
#1338=ORIENTED_EDGE('',*,*,#998,.T.);
#1339=ORIENTED_EDGE('',*,*,#996,.T.);
#1340=ORIENTED_EDGE('',*,*,#998,.F.);
#1341=ORIENTED_EDGE('',*,*,#972,.T.);
#1342=ORIENTED_EDGE('',*,*,#999,.T.);
#1343=ORIENTED_EDGE('',*,*,#1000,.F.);
#1344=ORIENTED_EDGE('',*,*,#999,.F.);
#1345=ORIENTED_EDGE('',*,*,#1000,.T.);
#1346=ORIENTED_EDGE('',*,*,#1001,.F.);
#1347=ORIENTED_EDGE('',*,*,#1002,.F.);
#1348=ORIENTED_EDGE('',*,*,#1003,.T.);
#1349=ORIENTED_EDGE('',*,*,#1001,.T.);
#1350=ORIENTED_EDGE('',*,*,#1003,.F.);
#1351=ORIENTED_EDGE('',*,*,#1004,.F.);
#1352=ORIENTED_EDGE('',*,*,#1005,.T.);
#1353=ORIENTED_EDGE('',*,*,#1002,.T.);
#1354=ORIENTED_EDGE('',*,*,#1005,.F.);
#1355=ORIENTED_EDGE('',*,*,#1004,.T.);
#1356=ORIENTED_EDGE('',*,*,#1006,.T.);
#1357=ORIENTED_EDGE('',*,*,#997,.F.);
#1358=ORIENTED_EDGE('',*,*,#1006,.F.);
#1359=ORIENTED_EDGE('',*,*,#1007,.F.);
#1360=ORIENTED_EDGE('',*,*,#1008,.F.);
#1361=ORIENTED_EDGE('',*,*,#1009,.F.);
#1362=ORIENTED_EDGE('',*,*,#1010,.T.);
#1363=ORIENTED_EDGE('',*,*,#1011,.F.);
#1364=ORIENTED_EDGE('',*,*,#1012,.T.);
#1365=ORIENTED_EDGE('',*,*,#1013,.F.);
#1366=ORIENTED_EDGE('',*,*,#1014,.F.);
#1367=ORIENTED_EDGE('',*,*,#1015,.F.);
#1368=ORIENTED_EDGE('',*,*,#1010,.F.);
#1369=ORIENTED_EDGE('',*,*,#1016,.F.);
#1370=ORIENTED_EDGE('',*,*,#1017,.F.);
#1371=ORIENTED_EDGE('',*,*,#1018,.F.);
#1372=ORIENTED_EDGE('',*,*,#1019,.F.);
#1373=ORIENTED_EDGE('',*,*,#1017,.T.);
#1374=ORIENTED_EDGE('',*,*,#1020,.F.);
#1375=ORIENTED_EDGE('',*,*,#1021,.F.);
#1376=ORIENTED_EDGE('',*,*,#1022,.F.);
#1377=ORIENTED_EDGE('',*,*,#1023,.T.);
#1378=ORIENTED_EDGE('',*,*,#1024,.F.);
#1379=ORIENTED_EDGE('',*,*,#1025,.F.);
#1380=ORIENTED_EDGE('',*,*,#1026,.F.);
#1381=ORIENTED_EDGE('',*,*,#1021,.T.);
#1382=ORIENTED_EDGE('',*,*,#1027,.F.);
#1383=ORIENTED_EDGE('',*,*,#1023,.F.);
#1384=ORIENTED_EDGE('',*,*,#1028,.F.);
#1385=ORIENTED_EDGE('',*,*,#1029,.F.);
#1386=ORIENTED_EDGE('',*,*,#1030,.F.);
#1387=ORIENTED_EDGE('',*,*,#1031,.F.);
#1388=ORIENTED_EDGE('',*,*,#1032,.T.);
#1389=ORIENTED_EDGE('',*,*,#1033,.F.);
#1390=ORIENTED_EDGE('',*,*,#1034,.F.);
#1391=ORIENTED_EDGE('',*,*,#1032,.F.);
#1392=ORIENTED_EDGE('',*,*,#1035,.F.);
#1393=ORIENTED_EDGE('',*,*,#1036,.T.);
#1394=ORIENTED_EDGE('',*,*,#1037,.F.);
#1395=ORIENTED_EDGE('',*,*,#1036,.F.);
#1396=ORIENTED_EDGE('',*,*,#1038,.F.);
#1397=ORIENTED_EDGE('',*,*,#1039,.F.);
#1398=ORIENTED_EDGE('',*,*,#1040,.T.);
#1399=ORIENTED_EDGE('',*,*,#1041,.F.);
#1400=ORIENTED_EDGE('',*,*,#1042,.F.);
#1401=ORIENTED_EDGE('',*,*,#1043,.F.);
#1402=ORIENTED_EDGE('',*,*,#1040,.F.);
#1403=ORIENTED_EDGE('',*,*,#1044,.F.);
#1404=ORIENTED_EDGE('',*,*,#1012,.F.);
#1405=ORIENTED_EDGE('',*,*,#1045,.F.);
#1406=ORIENTED_EDGE('',*,*,#1046,.T.);
#1407=ORIENTED_EDGE('',*,*,#1041,.T.);
#1408=ORIENTED_EDGE('',*,*,#1043,.T.);
#1409=ORIENTED_EDGE('',*,*,#1047,.T.);
#1410=ORIENTED_EDGE('',*,*,#1018,.T.);
#1411=ORIENTED_EDGE('',*,*,#1019,.T.);
#1412=ORIENTED_EDGE('',*,*,#1026,.T.);
#1413=ORIENTED_EDGE('',*,*,#1048,.T.);
#1414=ORIENTED_EDGE('',*,*,#1033,.T.);
#1415=ORIENTED_EDGE('',*,*,#1037,.T.);
#1416=ORIENTED_EDGE('',*,*,#1046,.F.);
#1417=ORIENTED_EDGE('',*,*,#1039,.T.);
#1418=ORIENTED_EDGE('',*,*,#1049,.T.);
#1419=ORIENTED_EDGE('',*,*,#1050,.T.);
#1420=ORIENTED_EDGE('',*,*,#1049,.F.);
#1421=ORIENTED_EDGE('',*,*,#1038,.T.);
#1422=ORIENTED_EDGE('',*,*,#1035,.T.);
#1423=ORIENTED_EDGE('',*,*,#1031,.T.);
#1424=ORIENTED_EDGE('',*,*,#1051,.F.);
#1425=ORIENTED_EDGE('',*,*,#1024,.T.);
#1426=ORIENTED_EDGE('',*,*,#1027,.T.);
#1427=ORIENTED_EDGE('',*,*,#1020,.T.);
#1428=ORIENTED_EDGE('',*,*,#1016,.T.);
#1429=ORIENTED_EDGE('',*,*,#1009,.T.);
#1430=ORIENTED_EDGE('',*,*,#1052,.F.);
#1431=ORIENTED_EDGE('',*,*,#1013,.T.);
#1432=ORIENTED_EDGE('',*,*,#1044,.T.);
#1433=ORIENTED_EDGE('',*,*,#1034,.T.);
#1434=ORIENTED_EDGE('',*,*,#1048,.F.);
#1435=ORIENTED_EDGE('',*,*,#1028,.T.);
#1436=ORIENTED_EDGE('',*,*,#1022,.T.);
#1437=ORIENTED_EDGE('',*,*,#1053,.T.);
#1438=ORIENTED_EDGE('',*,*,#1029,.T.);
#1439=ORIENTED_EDGE('',*,*,#1042,.T.);
#1440=ORIENTED_EDGE('',*,*,#1011,.T.);
#1441=ORIENTED_EDGE('',*,*,#1054,.T.);
#1442=ORIENTED_EDGE('',*,*,#1007,.T.);
#1443=ORIENTED_EDGE('',*,*,#1015,.T.);
#1444=ORIENTED_EDGE('',*,*,#1047,.F.);
#1445=ORIENTED_EDGE('',*,*,#1030,.T.);
#1446=ORIENTED_EDGE('',*,*,#1053,.F.);
#1447=ORIENTED_EDGE('',*,*,#1025,.T.);
#1448=ORIENTED_EDGE('',*,*,#1051,.T.);
#1449=ORIENTED_EDGE('',*,*,#1014,.T.);
#1450=ORIENTED_EDGE('',*,*,#1052,.T.);
#1451=ORIENTED_EDGE('',*,*,#1008,.T.);
#1452=ORIENTED_EDGE('',*,*,#1054,.F.);
#1453=ORIENTED_EDGE('',*,*,#1055,.T.);
#1454=ORIENTED_EDGE('',*,*,#1050,.F.);
#1455=ORIENTED_EDGE('',*,*,#1056,.F.);
#1456=ORIENTED_EDGE('',*,*,#1057,.T.);
#1457=ORIENTED_EDGE('',*,*,#1045,.T.);
#1458=ORIENTED_EDGE('',*,*,#1057,.F.);
#1459=ORIENTED_EDGE('',*,*,#1058,.F.);
#1460=ORIENTED_EDGE('',*,*,#1059,.T.);
#1461=ORIENTED_EDGE('',*,*,#1056,.T.);
#1462=ORIENTED_EDGE('',*,*,#1059,.F.);
#1463=ORIENTED_EDGE('',*,*,#1060,.F.);
#1464=ORIENTED_EDGE('',*,*,#1061,.T.);
#1465=ORIENTED_EDGE('',*,*,#1058,.T.);
#1466=ORIENTED_EDGE('',*,*,#1061,.F.);
#1467=ORIENTED_EDGE('',*,*,#1060,.T.);
#1468=ORIENTED_EDGE('',*,*,#1062,.T.);
#1469=ORIENTED_EDGE('',*,*,#1063,.F.);
#1470=ORIENTED_EDGE('',*,*,#1062,.F.);
#1471=ORIENTED_EDGE('',*,*,#1063,.T.);
#1472=ORIENTED_EDGE('',*,*,#1064,.F.);
#1473=ORIENTED_EDGE('',*,*,#1055,.F.);
#1474=ORIENTED_EDGE('',*,*,#1065,.T.);
#1475=ORIENTED_EDGE('',*,*,#1064,.T.);
#1476=ORIENTED_EDGE('',*,*,#1065,.F.);
#1477=ORIENTED_EDGE('',*,*,#1066,.T.);
#1478=ORIENTED_EDGE('',*,*,#1067,.T.);
#1479=ORIENTED_EDGE('',*,*,#1068,.T.);
#1480=ORIENTED_EDGE('',*,*,#1067,.F.);
#1481=ORIENTED_EDGE('',*,*,#1066,.F.);
#1482=ORIENTED_EDGE('',*,*,#1069,.T.);
#1483=ORIENTED_EDGE('',*,*,#1070,.T.);
#1484=ORIENTED_EDGE('',*,*,#1069,.F.);
#1485=ORIENTED_EDGE('',*,*,#1068,.F.);
#1486=ORIENTED_EDGE('',*,*,#1070,.F.);
#1487=SPHERICAL_SURFACE('',#1693,1.78305659323844);
#1488=ADVANCED_FACE('',(#403),#1487,.T.);
#1489=ADVANCED_FACE('',(#404),#331,.F.);
#1490=ADVANCED_FACE('',(#405),#91,.T.);
#1491=ADVANCED_FACE('',(#406),#332,.F.);
#1492=ADVANCED_FACE('',(#407),#92,.T.);
#1493=ADVANCED_FACE('',(#408),#333,.F.);
#1494=ADVANCED_FACE('',(#409),#93,.T.);
#1495=ADVANCED_FACE('',(#410,#67),#94,.T.);
#1496=ADVANCED_FACE('',(#411),#334,.F.);
#1497=ADVANCED_FACE('',(#412),#48,.F.);
#1498=ADVANCED_FACE('',(#413),#335,.F.);
#1499=ADVANCED_FACE('',(#414,#68),#95,.T.);
#1500=ADVANCED_FACE('',(#415),#336,.T.);
#1501=ADVANCED_FACE('',(#416,#69),#96,.T.);
#1502=ADVANCED_FACE('',(#417),#337,.F.);
#1503=ADVANCED_FACE('',(#418,#70),#97,.T.);
#1504=ADVANCED_FACE('',(#419),#338,.F.);
#1505=ADVANCED_FACE('',(#420),#98,.T.);
#1506=ADVANCED_FACE('',(#421),#339,.T.);
#1507=ADVANCED_FACE('',(#422),#49,.T.);
#1508=ADVANCED_FACE('',(#423,#71),#99,.T.);
#1509=ADVANCED_FACE('',(#424),#50,.F.);
#1510=ADVANCED_FACE('',(#425,#72),#100,.T.);
#1511=ADVANCED_FACE('',(#426),#340,.F.);
#1512=ADVANCED_FACE('',(#427,#73),#101,.T.);
#1513=ADVANCED_FACE('',(#428),#341,.F.);
#1514=ADVANCED_FACE('',(#429,#74),#102,.T.);
#1515=ADVANCED_FACE('',(#430),#342,.F.);
#1516=ADVANCED_FACE('',(#431),#51,.F.);
#1517=ADVANCED_FACE('',(#432),#343,.F.);
#1518=ADVANCED_FACE('',(#433),#52,.F.);
#1519=ADVANCED_FACE('',(#434,#75),#103,.T.);
#1520=ADVANCED_FACE('',(#435),#53,.T.);
#1521=ADVANCED_FACE('',(#436),#344,.T.);
#1522=ADVANCED_FACE('',(#437,#76),#104,.T.);
#1523=ADVANCED_FACE('',(#438),#54,.T.);
#1524=ADVANCED_FACE('',(#439),#55,.T.);
#1525=ADVANCED_FACE('',(#440),#345,.T.);
#1526=ADVANCED_FACE('',(#441,#77),#105,.T.);
#1527=ADVANCED_FACE('',(#442),#56,.T.);
#1528=ADVANCED_FACE('',(#443),#346,.T.);
#1529=ADVANCED_FACE('',(#444),#57,.T.);
#1530=ADVANCED_FACE('',(#445,#78),#106,.T.);
#1531=ADVANCED_FACE('',(#446),#347,.F.);
#1532=ADVANCED_FACE('',(#447),#107,.T.);
#1533=ADVANCED_FACE('',(#448),#108,.T.);
#1534=ADVANCED_FACE('',(#449),#348,.T.);
#1535=ADVANCED_FACE('',(#450,#79),#109,.T.);
#1536=ADVANCED_FACE('',(#451),#349,.T.);
#1537=ADVANCED_FACE('',(#452),#58,.T.);
#1538=ADVANCED_FACE('',(#453),#350,.T.);
#1539=ADVANCED_FACE('',(#454,#80),#110,.T.);
#1540=ADVANCED_FACE('',(#455),#351,.T.);
#1541=ADVANCED_FACE('',(#456,#81),#111,.T.);
#1542=ADVANCED_FACE('',(#457),#352,.T.);
#1543=ADVANCED_FACE('',(#458,#82),#112,.T.);
#1544=ADVANCED_FACE('',(#459),#59,.F.);
#1545=ADVANCED_FACE('',(#460),#353,.F.);
#1546=ADVANCED_FACE('',(#461,#83),#113,.T.);
#1547=ADVANCED_FACE('',(#462),#44,.T.);
#1548=ADVANCED_FACE('',(#463,#84,#85,#86),#354,.T.);
#1549=ADVANCED_FACE('',(#464),#355,.F.);
#1550=ADVANCED_FACE('',(#465),#45,.T.);
#1551=ADVANCED_FACE('',(#466),#356,.F.);
#1552=ADVANCED_FACE('',(#467),#46,.T.);
#1553=ADVANCED_FACE('',(#468),#357,.F.);
#1554=ADVANCED_FACE('',(#469),#114,.F.);
#1555=ADVANCED_FACE('',(#470),#115,.F.);
#1556=ADVANCED_FACE('',(#471),#116,.F.);
#1557=ADVANCED_FACE('',(#472),#47,.T.);
#1558=ADVANCED_FACE('',(#473),#358,.F.);
#1559=ADVANCED_FACE('',(#474),#117,.F.);
#1560=ADVANCED_FACE('',(#475,#87),#118,.T.);
#1561=ADVANCED_FACE('',(#476),#60,.T.);
#1562=ADVANCED_FACE('',(#477),#61,.T.);
#1563=ADVANCED_FACE('',(#478,#88),#119,.T.);
#1564=ADVANCED_FACE('',(#479),#62,.F.);
#1565=ADVANCED_FACE('',(#480),#359,.F.);
#1566=ADVANCED_FACE('',(#481),#63,.F.);
#1567=ADVANCED_FACE('',(#482),#120,.F.);
#1568=ADVANCED_FACE('',(#483),#121,.F.);
#1569=ADVANCED_FACE('',(#484),#360,.F.);
#1570=ADVANCED_FACE('',(#485),#122,.F.);
#1571=ADVANCED_FACE('',(#486),#123,.F.);
#1572=ADVANCED_FACE('',(#487),#361,.F.);
#1573=ADVANCED_FACE('',(#488),#124,.F.);
#1574=ADVANCED_FACE('',(#489),#362,.F.);
#1575=ADVANCED_FACE('',(#490),#125,.F.);
#1576=ADVANCED_FACE('',(#491),#363,.F.);
#1577=ADVANCED_FACE('',(#492),#43,.F.);
#1578=ADVANCED_FACE('',(#493),#364,.F.);
#1579=ADVANCED_FACE('',(#494),#365,.T.);
#1580=ADVANCED_FACE('',(#495),#366,.T.);
#1581=ADVANCED_FACE('',(#496),#126,.T.);
#1582=ADVANCED_FACE('',(#497),#127,.T.);
#1583=ADVANCED_FACE('',(#498,#89),#128,.T.);
#1584=ADVANCED_FACE('',(#499),#367,.T.);
#1585=ADVANCED_FACE('',(#500),#64,.T.);
#1586=ADVANCED_FACE('',(#501),#368,.T.);
#1587=ADVANCED_FACE('',(#502),#65,.T.);
#1588=ADVANCED_FACE('',(#503,#90),#129,.T.);
#1589=ADVANCED_FACE('',(#504),#369,.F.);
#1590=ADVANCED_FACE('',(#505),#66,.T.);
#1591=ADVANCED_FACE('',(#506),#370,.T.);
#1592=ADVANCED_FACE('',(#507),#130,.T.);
#1593=ADVANCED_FACE('',(#508),#131,.F.);
#1594=CLOSED_SHELL('',(#1488));
#1595=CLOSED_SHELL('',(#1489,#1490,#1491,#1492,#1493,#1494,#1495,#1496,
#1497,#1498,#1499,#1500,#1501,#1502,#1503,#1504,#1505));
#1596=CLOSED_SHELL('',(#1506,#1507,#1508,#1509,#1510,#1511,#1512,#1513,
#1514,#1515,#1516,#1517,#1518,#1519,#1520,#1521,#1522,#1523));
#1597=CLOSED_SHELL('',(#1524,#1525,#1526,#1527,#1528,#1529,#1530,#1531,
#1532,#1533,#1534,#1535,#1536));
#1598=CLOSED_SHELL('',(#1537,#1538,#1539,#1540,#1541,#1542,#1543,#1544,
#1545,#1546));
#1599=CLOSED_SHELL('',(#1547,#1548,#1549,#1550,#1551,#1552,#1553,#1554,
#1555,#1556,#1557,#1558,#1559,#1560,#1561,#1562,#1563,#1564,#1565,#1566));
#1600=CLOSED_SHELL('',(#1567,#1568,#1569,#1570,#1571,#1572,#1573,#1574,
#1575,#1576,#1577,#1578,#1579,#1580,#1581,#1582,#1583,#1584,#1585,#1586,
#1587,#1588,#1589));
#1601=CLOSED_SHELL('',(#1590,#1591,#1592,#1593));
#1602=DERIVED_UNIT_ELEMENT(#1618,1.);
#1603=DERIVED_UNIT_ELEMENT(#4615,-3.);
#1604=DERIVED_UNIT_ELEMENT(#1618,1.);
#1605=DERIVED_UNIT_ELEMENT(#4615,-3.);
#1606=DERIVED_UNIT_ELEMENT(#1618,1.);
#1607=DERIVED_UNIT_ELEMENT(#4615,-3.);
#1608=DERIVED_UNIT_ELEMENT(#1618,1.);
#1609=DERIVED_UNIT_ELEMENT(#4615,-3.);
#1610=DERIVED_UNIT_ELEMENT(#1618,1.);
#1611=DERIVED_UNIT_ELEMENT(#4615,-3.);
#1612=DERIVED_UNIT_ELEMENT(#1618,1.);
#1613=DERIVED_UNIT_ELEMENT(#4615,-3.);
#1614=DERIVED_UNIT_ELEMENT(#1618,1.);
#1615=DERIVED_UNIT_ELEMENT(#4615,-3.);
#1616=DERIVED_UNIT_ELEMENT(#1618,1.);
#1617=DERIVED_UNIT_ELEMENT(#4615,-3.);
#1618=(
MASS_UNIT()
NAMED_UNIT(*)
SI_UNIT(.KILO.,.GRAM.)
);
#1619=DERIVED_UNIT((#1602,#1603));
#1620=DERIVED_UNIT((#1604,#1605));
#1621=DERIVED_UNIT((#1606,#1607));
#1622=DERIVED_UNIT((#1608,#1609));
#1623=DERIVED_UNIT((#1610,#1611));
#1624=DERIVED_UNIT((#1612,#1613));
#1625=DERIVED_UNIT((#1614,#1615));
#1626=DERIVED_UNIT((#1616,#1617));
#1627=MEASURE_REPRESENTATION_ITEM('density measure',
POSITIVE_RATIO_MEASURE(7850.),#1619);
#1628=MEASURE_REPRESENTATION_ITEM('density measure',
POSITIVE_RATIO_MEASURE(7850.),#1620);
#1629=MEASURE_REPRESENTATION_ITEM('density measure',
POSITIVE_RATIO_MEASURE(7850.),#1621);
#1630=MEASURE_REPRESENTATION_ITEM('density measure',
POSITIVE_RATIO_MEASURE(7850.),#1622);
#1631=MEASURE_REPRESENTATION_ITEM('density measure',
POSITIVE_RATIO_MEASURE(7850.),#1623);
#1632=MEASURE_REPRESENTATION_ITEM('density measure',
POSITIVE_RATIO_MEASURE(7850.),#1624);
#1633=MEASURE_REPRESENTATION_ITEM('density measure',
POSITIVE_RATIO_MEASURE(7850.),#1625);
#1634=MEASURE_REPRESENTATION_ITEM('density measure',
POSITIVE_RATIO_MEASURE(7850.),#1626);
#1635=PROPERTY_DEFINITION_REPRESENTATION(#1675,#1651);
#1636=PROPERTY_DEFINITION_REPRESENTATION(#1676,#1652);
#1637=PROPERTY_DEFINITION_REPRESENTATION(#1677,#1653);
#1638=PROPERTY_DEFINITION_REPRESENTATION(#1678,#1654);
#1639=PROPERTY_DEFINITION_REPRESENTATION(#1679,#1655);
#1640=PROPERTY_DEFINITION_REPRESENTATION(#1680,#1656);
#1641=PROPERTY_DEFINITION_REPRESENTATION(#1681,#1657);
#1642=PROPERTY_DEFINITION_REPRESENTATION(#1682,#1658);
#1643=PROPERTY_DEFINITION_REPRESENTATION(#1683,#1659);
#1644=PROPERTY_DEFINITION_REPRESENTATION(#1684,#1660);
#1645=PROPERTY_DEFINITION_REPRESENTATION(#1685,#1661);
#1646=PROPERTY_DEFINITION_REPRESENTATION(#1686,#1662);
#1647=PROPERTY_DEFINITION_REPRESENTATION(#1687,#1663);
#1648=PROPERTY_DEFINITION_REPRESENTATION(#1688,#1664);
#1649=PROPERTY_DEFINITION_REPRESENTATION(#1689,#1665);
#1650=PROPERTY_DEFINITION_REPRESENTATION(#1690,#1666);
#1651=REPRESENTATION('material name',(#1667),#4605);
#1652=REPRESENTATION('density',(#1627),#4605);
#1653=REPRESENTATION('material name',(#1668),#4606);
#1654=REPRESENTATION('density',(#1628),#4606);
#1655=REPRESENTATION('material name',(#1669),#4607);
#1656=REPRESENTATION('density',(#1629),#4607);
#1657=REPRESENTATION('material name',(#1670),#4608);
#1658=REPRESENTATION('density',(#1630),#4608);
#1659=REPRESENTATION('material name',(#1671),#4609);
#1660=REPRESENTATION('density',(#1631),#4609);
#1661=REPRESENTATION('material name',(#1672),#4610);
#1662=REPRESENTATION('density',(#1632),#4610);
#1663=REPRESENTATION('material name',(#1673),#4611);
#1664=REPRESENTATION('density',(#1633),#4611);
#1665=REPRESENTATION('material name',(#1674),#4612);
#1666=REPRESENTATION('density',(#1634),#4612);
#1667=DESCRIPTIVE_REPRESENTATION_ITEM('Steel','Steel');
#1668=DESCRIPTIVE_REPRESENTATION_ITEM('Steel','Steel');
#1669=DESCRIPTIVE_REPRESENTATION_ITEM('Steel','Steel');
#1670=DESCRIPTIVE_REPRESENTATION_ITEM('Steel','Steel');
#1671=DESCRIPTIVE_REPRESENTATION_ITEM('Steel','Steel');
#1672=DESCRIPTIVE_REPRESENTATION_ITEM('Steel','Steel');
#1673=DESCRIPTIVE_REPRESENTATION_ITEM('Steel','Steel');
#1674=DESCRIPTIVE_REPRESENTATION_ITEM('Steel','Steel');
#1675=PROPERTY_DEFINITION('material property','material name',#4655);
#1676=PROPERTY_DEFINITION('material property','density of part',#4655);
#1677=PROPERTY_DEFINITION('material property','material name',#4656);
#1678=PROPERTY_DEFINITION('material property','density of part',#4656);
#1679=PROPERTY_DEFINITION('material property','material name',#4657);
#1680=PROPERTY_DEFINITION('material property','density of part',#4657);
#1681=PROPERTY_DEFINITION('material property','material name',#4658);
#1682=PROPERTY_DEFINITION('material property','density of part',#4658);
#1683=PROPERTY_DEFINITION('material property','material name',#4659);
#1684=PROPERTY_DEFINITION('material property','density of part',#4659);
#1685=PROPERTY_DEFINITION('material property','material name',#4660);
#1686=PROPERTY_DEFINITION('material property','density of part',#4660);
#1687=PROPERTY_DEFINITION('material property','material name',#4661);
#1688=PROPERTY_DEFINITION('material property','density of part',#4661);
#1689=PROPERTY_DEFINITION('material property','material name',#4662);
#1690=PROPERTY_DEFINITION('material property','density of part',#4662);
#1691=AXIS2_PLACEMENT_3D('',#2407,#1902,#1903);
#1692=AXIS2_PLACEMENT_3D('',#2408,#1904,#1905);
#1693=AXIS2_PLACEMENT_3D('',#2409,#1906,#1907);
#1694=AXIS2_PLACEMENT_3D('',#2412,#1908,#1909);
#1695=AXIS2_PLACEMENT_3D('',#2413,#1910,#1911);
#1696=AXIS2_PLACEMENT_3D('',#2414,#1912,#1913);
#1697=AXIS2_PLACEMENT_3D('',#2419,#1915,#1916);
#1698=AXIS2_PLACEMENT_3D('',#2516,#1921,#1922);
#1699=AXIS2_PLACEMENT_3D('',#2518,#1924,#1925);
#1700=AXIS2_PLACEMENT_3D('',#2520,#1926,#1927);
#1701=AXIS2_PLACEMENT_3D('',#2522,#1929,#1930);
#1702=AXIS2_PLACEMENT_3D('',#2523,#1931,#1932);
#1703=AXIS2_PLACEMENT_3D('',#2524,#1933,#1934);
#1704=AXIS2_PLACEMENT_3D('',#2525,#1935,#1936);
#1705=AXIS2_PLACEMENT_3D('',#2526,#1937,#1938);
#1706=AXIS2_PLACEMENT_3D('',#2527,#1939,#1940);
#1707=AXIS2_PLACEMENT_3D('',#2528,#1941,#1942);
#1708=AXIS2_PLACEMENT_3D('',#2530,#1943,#1944);
#1709=AXIS2_PLACEMENT_3D('',#2531,#1945,#1946);
#1710=AXIS2_PLACEMENT_3D('',#2533,#1947,#1948);
#1711=AXIS2_PLACEMENT_3D('',#2535,#1950,#1951);
#1712=AXIS2_PLACEMENT_3D('',#2538,#1953,#1954);
#1713=AXIS2_PLACEMENT_3D('',#2539,#1955,#1956);
#1714=AXIS2_PLACEMENT_3D('',#2541,#1957,#1958);
#1715=AXIS2_PLACEMENT_3D('',#2543,#1960,#1961);
#1716=AXIS2_PLACEMENT_3D('',#2545,#1962,#1963);
#1717=AXIS2_PLACEMENT_3D('',#2546,#1964,#1965);
#1718=AXIS2_PLACEMENT_3D('',#2548,#1966,#1967);
#1719=AXIS2_PLACEMENT_3D('',#2551,#1970,#1971);
#1720=AXIS2_PLACEMENT_3D('',#2553,#1972,#1973);
#1721=AXIS2_PLACEMENT_3D('',#2554,#1974,#1975);
#1722=AXIS2_PLACEMENT_3D('',#2556,#1976,#1977);
#1723=AXIS2_PLACEMENT_3D('',#2558,#1979,#1980);
#1724=AXIS2_PLACEMENT_3D('',#2560,#1981,#1982);
#1725=AXIS2_PLACEMENT_3D('',#2561,#1983,#1984);
#1726=AXIS2_PLACEMENT_3D('',#2563,#1985,#1986);
#1727=AXIS2_PLACEMENT_3D('',#2565,#1988,#1989);
#1728=AXIS2_PLACEMENT_3D('',#2566,#1990,#1991);
#1729=AXIS2_PLACEMENT_3D('',#2567,#1992,#1993);
#1730=AXIS2_PLACEMENT_3D('',#2569,#1994,#1995);
#1731=AXIS2_PLACEMENT_3D('',#2572,#1997,#1998);
#1732=AXIS2_PLACEMENT_3D('',#2573,#1999,#2000);
#1733=AXIS2_PLACEMENT_3D('',#2576,#2002,#2003);
#1734=AXIS2_PLACEMENT_3D('',#2577,#2004,#2005);
#1735=AXIS2_PLACEMENT_3D('',#2579,#2006,#2007);
#1736=AXIS2_PLACEMENT_3D('',#2580,#2008,#2009);
#1737=AXIS2_PLACEMENT_3D('',#2582,#2010,#2011);
#1738=AXIS2_PLACEMENT_3D('',#2584,#2013,#2014);
#1739=AXIS2_PLACEMENT_3D('',#2586,#2015,#2016);
#1740=AXIS2_PLACEMENT_3D('',#2587,#2017,#2018);
#1741=AXIS2_PLACEMENT_3D('',#2589,#2019,#2020);
#1742=AXIS2_PLACEMENT_3D('',#2591,#2022,#2023);
#1743=AXIS2_PLACEMENT_3D('',#2593,#2024,#2025);
#1744=AXIS2_PLACEMENT_3D('',#2594,#2026,#2027);
#1745=AXIS2_PLACEMENT_3D('',#2596,#2028,#2029);
#1746=AXIS2_PLACEMENT_3D('',#2598,#2031,#2032);
#1747=AXIS2_PLACEMENT_3D('',#2600,#2033,#2034);
#1748=AXIS2_PLACEMENT_3D('',#2601,#2035,#2036);
#1749=AXIS2_PLACEMENT_3D('',#2603,#2037,#2038);
#1750=AXIS2_PLACEMENT_3D('',#2605,#2040,#2041);
#1751=AXIS2_PLACEMENT_3D('',#2608,#2043,#2044);
#1752=AXIS2_PLACEMENT_3D('',#2609,#2045,#2046);
#1753=AXIS2_PLACEMENT_3D('',#2611,#2047,#2048);
#1754=AXIS2_PLACEMENT_3D('',#2613,#2050,#2051);
#1755=AXIS2_PLACEMENT_3D('',#2616,#2053,#2054);
#1756=AXIS2_PLACEMENT_3D('',#2617,#2055,#2056);
#1757=AXIS2_PLACEMENT_3D('',#2619,#2057,#2058);
#1758=AXIS2_PLACEMENT_3D('',#2620,#2059,#2060);
#1759=AXIS2_PLACEMENT_3D('',#2622,#2061,#2062);
#1760=AXIS2_PLACEMENT_3D('',#2624,#2064,#2065);
#1761=AXIS2_PLACEMENT_3D('',#2626,#2066,#2067);
#1762=AXIS2_PLACEMENT_3D('',#2628,#2069,#2070);
#1763=AXIS2_PLACEMENT_3D('',#2630,#2071,#2072);
#1764=AXIS2_PLACEMENT_3D('',#2631,#2073,#2074);
#1765=AXIS2_PLACEMENT_3D('',#2633,#2076,#2077);
#1766=AXIS2_PLACEMENT_3D('',#2634,#2078,#2079);
#1767=AXIS2_PLACEMENT_3D('',#2636,#2080,#2081);
#1768=AXIS2_PLACEMENT_3D('',#2639,#2083,#2084);
#1769=AXIS2_PLACEMENT_3D('',#2640,#2085,#2086);
#1770=AXIS2_PLACEMENT_3D('',#2642,#2087,#2088);
#1771=AXIS2_PLACEMENT_3D('',#2644,#2090,#2091);
#1772=AXIS2_PLACEMENT_3D('',#2646,#2092,#2093);
#1773=AXIS2_PLACEMENT_3D('',#2647,#2094,#2095);
#1774=AXIS2_PLACEMENT_3D('',#2649,#2096,#2097);
#1775=AXIS2_PLACEMENT_3D('',#2651,#2099,#2100);
#1776=AXIS2_PLACEMENT_3D('',#2653,#2101,#2102);
#1777=AXIS2_PLACEMENT_3D('',#2655,#2104,#2105);
#1778=AXIS2_PLACEMENT_3D('',#2658,#2107,#2108);
#1779=AXIS2_PLACEMENT_3D('',#2659,#2109,#2110);
#1780=AXIS2_PLACEMENT_3D('',#2661,#2111,#2112);
#1781=AXIS2_PLACEMENT_3D('',#2662,#2113,#2114);
#1782=AXIS2_PLACEMENT_3D('',#2664,#2115,#2116);
#1783=AXIS2_PLACEMENT_3D('',#2666,#2118,#2119);
#1784=AXIS2_PLACEMENT_3D('',#2667,#2120,#2121);
#1785=AXIS2_PLACEMENT_3D('',#2669,#2122,#2123);
#1786=AXIS2_PLACEMENT_3D('',#2670,#2124,#2125);
#1787=AXIS2_PLACEMENT_3D('',#2672,#2126,#2127);
#1788=AXIS2_PLACEMENT_3D('',#2674,#2129,#2130);
#1789=AXIS2_PLACEMENT_3D('',#2676,#2131,#2132);
#1790=AXIS2_PLACEMENT_3D('',#2677,#2133,#2134);
#1791=AXIS2_PLACEMENT_3D('',#2679,#2136,#2137);
#1792=AXIS2_PLACEMENT_3D('',#2680,#2138,#2139);
#1793=AXIS2_PLACEMENT_3D('',#2682,#2140,#2141);
#1794=AXIS2_PLACEMENT_3D('',#2685,#2143,#2144);
#1795=AXIS2_PLACEMENT_3D('',#2686,#2145,#2146);
#1796=AXIS2_PLACEMENT_3D('',#2688,#2147,#2148);
#1797=AXIS2_PLACEMENT_3D('',#2690,#2150,#2151);
#1798=AXIS2_PLACEMENT_3D('',#2692,#2152,#2153);
#1799=AXIS2_PLACEMENT_3D('',#2693,#2154,#2155);
#1800=AXIS2_PLACEMENT_3D('',#2695,#2156,#2157);
#1801=AXIS2_PLACEMENT_3D('',#2697,#2159,#2160);
#1802=AXIS2_PLACEMENT_3D('',#2699,#2161,#2162);
#1803=AXIS2_PLACEMENT_3D('',#2700,#2163,#2164);
#1804=AXIS2_PLACEMENT_3D('',#2702,#2165,#2166);
#1805=AXIS2_PLACEMENT_3D('',#2704,#2168,#2169);
#1806=AXIS2_PLACEMENT_3D('',#2706,#2170,#2171);
#1807=AXIS2_PLACEMENT_3D('',#2707,#2172,#2173);
#1808=AXIS2_PLACEMENT_3D('',#2709,#2174,#2175);
#1809=AXIS2_PLACEMENT_3D('',#2711,#2177,#2178);
#1810=AXIS2_PLACEMENT_3D('',#2713,#2179,#2180);
#1811=AXIS2_PLACEMENT_3D('',#2715,#2182,#2183);
#1812=AXIS2_PLACEMENT_3D('',#2716,#2184,#2185);
#1813=AXIS2_PLACEMENT_3D('',#2975,#2187,#2188);
#1814=AXIS2_PLACEMENT_3D('',#2977,#2189,#2190);
#1815=AXIS2_PLACEMENT_3D('',#2981,#2193,#2194);
#1816=AXIS2_PLACEMENT_3D('',#3465,#2195,#2196);
#1817=AXIS2_PLACEMENT_3D('',#3467,#2197,#2198);
#1818=AXIS2_PLACEMENT_3D('',#3824,#2201,#2202);
#1819=AXIS2_PLACEMENT_3D('',#3826,#2203,#2204);
#1820=AXIS2_PLACEMENT_3D('',#4123,#2207,#2208);
#1821=AXIS2_PLACEMENT_3D('',#4125,#2209,#2210);
#1822=AXIS2_PLACEMENT_3D('',#4127,#2212,#2213);
#1823=AXIS2_PLACEMENT_3D('',#4128,#2214,#2215);
#1824=AXIS2_PLACEMENT_3D('',#4129,#2216,#2217);
#1825=AXIS2_PLACEMENT_3D('',#4325,#2219,#2220);
#1826=AXIS2_PLACEMENT_3D('',#4327,#2221,#2222);
#1827=AXIS2_PLACEMENT_3D('',#4329,#2224,#2225);
#1828=AXIS2_PLACEMENT_3D('',#4330,#2226,#2227);
#1829=AXIS2_PLACEMENT_3D('',#4332,#2228,#2229);
#1830=AXIS2_PLACEMENT_3D('',#4334,#2230,#2231);
#1831=AXIS2_PLACEMENT_3D('',#4335,#2232,#2233);
#1832=AXIS2_PLACEMENT_3D('',#4337,#2235,#2236);
#1833=AXIS2_PLACEMENT_3D('',#4340,#2238,#2239);
#1834=AXIS2_PLACEMENT_3D('',#4341,#2240,#2241);
#1835=AXIS2_PLACEMENT_3D('',#4343,#2242,#2243);
#1836=AXIS2_PLACEMENT_3D('',#4344,#2244,#2245);
#1837=AXIS2_PLACEMENT_3D('',#4346,#2246,#2247);
#1838=AXIS2_PLACEMENT_3D('',#4348,#2249,#2250);
#1839=AXIS2_PLACEMENT_3D('',#4350,#2251,#2252);
#1840=AXIS2_PLACEMENT_3D('',#4352,#2254,#2255);
#1841=AXIS2_PLACEMENT_3D('',#4354,#2257,#2258);
#1842=AXIS2_PLACEMENT_3D('',#4355,#2259,#2260);
#1843=AXIS2_PLACEMENT_3D('',#4364,#2265,#2266);
#1844=AXIS2_PLACEMENT_3D('',#4373,#2271,#2272);
#1845=AXIS2_PLACEMENT_3D('',#4407,#2274,#2275);
#1846=AXIS2_PLACEMENT_3D('',#4409,#2276,#2277);
#1847=AXIS2_PLACEMENT_3D('',#4411,#2278,#2279);
#1848=AXIS2_PLACEMENT_3D('',#4413,#2281,#2282);
#1849=AXIS2_PLACEMENT_3D('',#4422,#2287,#2288);
#1850=AXIS2_PLACEMENT_3D('',#4453,#2289,#2290);
#1851=AXIS2_PLACEMENT_3D('',#4462,#2295,#2296);
#1852=AXIS2_PLACEMENT_3D('',#4493,#2298,#2299);
#1853=AXIS2_PLACEMENT_3D('',#4495,#2300,#2301);
#1854=AXIS2_PLACEMENT_3D('',#4497,#2302,#2303);
#1855=AXIS2_PLACEMENT_3D('',#4499,#2304,#2305);
#1856=AXIS2_PLACEMENT_3D('',#4502,#2307,#2308);
#1857=AXIS2_PLACEMENT_3D('',#4503,#2309,#2310);
#1858=AXIS2_PLACEMENT_3D('',#4531,#2311,#2312);
#1859=AXIS2_PLACEMENT_3D('',#4533,#2313,#2314);
#1860=AXIS2_PLACEMENT_3D('',#4534,#2315,#2316);
#1861=AXIS2_PLACEMENT_3D('',#4535,#2317,#2318);
#1862=AXIS2_PLACEMENT_3D('',#4536,#2319,#2320);
#1863=AXIS2_PLACEMENT_3D('',#4537,#2321,#2322);
#1864=AXIS2_PLACEMENT_3D('',#4540,#2324,#2325);
#1865=AXIS2_PLACEMENT_3D('',#4541,#2326,#2327);
#1866=AXIS2_PLACEMENT_3D('',#4542,#2328,#2329);
#1867=AXIS2_PLACEMENT_3D('',#4543,#2330,#2331);
#1868=AXIS2_PLACEMENT_3D('',#4544,#2332,#2333);
#1869=AXIS2_PLACEMENT_3D('',#4545,#2334,#2335);
#1870=AXIS2_PLACEMENT_3D('',#4546,#2336,#2337);
#1871=AXIS2_PLACEMENT_3D('',#4547,#2338,#2339);
#1872=AXIS2_PLACEMENT_3D('',#4548,#2340,#2341);
#1873=AXIS2_PLACEMENT_3D('',#4549,#2342,#2343);
#1874=AXIS2_PLACEMENT_3D('',#4551,#2344,#2345);
#1875=AXIS2_PLACEMENT_3D('',#4552,#2346,#2347);
#1876=AXIS2_PLACEMENT_3D('',#4554,#2348,#2349);
#1877=AXIS2_PLACEMENT_3D('',#4556,#2351,#2352);
#1878=AXIS2_PLACEMENT_3D('',#4558,#2353,#2354);
#1879=AXIS2_PLACEMENT_3D('',#4560,#2356,#2357);
#1880=AXIS2_PLACEMENT_3D('',#4562,#2358,#2359);
#1881=AXIS2_PLACEMENT_3D('',#4564,#2361,#2362);
#1882=AXIS2_PLACEMENT_3D('',#4567,#2364,#2365);
#1883=AXIS2_PLACEMENT_3D('',#4568,#2366,#2367);
#1884=AXIS2_PLACEMENT_3D('',#4570,#2368,#2369);
#1885=AXIS2_PLACEMENT_3D('',#4571,#2370,#2371);
#1886=AXIS2_PLACEMENT_3D('',#4573,#2373,#2374);
#1887=AXIS2_PLACEMENT_3D('',#4574,#2375,#2376);
#1888=AXIS2_PLACEMENT_3D('',#4576,#2377,#2378);
#1889=AXIS2_PLACEMENT_3D('',#4579,#2380,#2381);
#1890=AXIS2_PLACEMENT_3D('',#4580,#2382,#2383);
#1891=AXIS2_PLACEMENT_3D('',#4583,#2385,#2386);
#1892=AXIS2_PLACEMENT_3D('',#4584,#2387,#2388);
#1893=AXIS2_PLACEMENT_3D('',#4585,#2389,#2390);
#1894=AXIS2_PLACEMENT_3D('',#4586,#2391,#2392);
#1895=AXIS2_PLACEMENT_3D('',#4587,#2393,#2394);
#1896=AXIS2_PLACEMENT_3D('',#4588,#2395,#2396);
#1897=AXIS2_PLACEMENT_3D('',#4589,#2397,#2398);
#1898=AXIS2_PLACEMENT_3D('',#4590,#2399,#2400);
#1899=AXIS2_PLACEMENT_3D('',#4591,#2401,#2402);
#1900=AXIS2_PLACEMENT_3D('',#4592,#2403,#2404);
#1901=AXIS2_PLACEMENT_3D('',#4593,#2405,#2406);
#1902=DIRECTION('axis',(0.,0.,1.));
#1903=DIRECTION('refdir',(1.,0.,0.));
#1904=DIRECTION('axis',(0.,0.,1.));
#1905=DIRECTION('refdir',(1.,0.,0.));
#1906=DIRECTION('center_axis',(1.,-1.22464679914735E-16,0.));
#1907=DIRECTION('ref_axis',(0.,-1.,0.));
#1908=DIRECTION('center_axis',(-7.49879891330929E-33,-1.22464679914735E-16,
1.));
#1909=DIRECTION('ref_axis',(0.,1.,1.22464679914735E-16));
#1910=DIRECTION('axis',(0.,0.,1.));
#1911=DIRECTION('refdir',(1.,0.,0.));
#1912=DIRECTION('center_axis',(0.,0.,1.));
#1913=DIRECTION('ref_axis',(1.,0.,0.));
#1914=DIRECTION('',(0.,0.,1.));
#1915=DIRECTION('center_axis',(0.,0.,-1.));
#1916=DIRECTION('ref_axis',(1.,0.,0.));
#1917=DIRECTION('',(0.,0.,-1.));
#1918=DIRECTION('',(0.,0.,-1.));
#1919=DIRECTION('',(0.,0.,1.));
#1920=DIRECTION('',(0.,0.,1.));
#1921=DIRECTION('center_axis',(0.,0.,1.));
#1922=DIRECTION('ref_axis',(1.,0.,0.));
#1923=DIRECTION('',(0.,1.,0.));
#1924=DIRECTION('center_axis',(1.,0.,0.));
#1925=DIRECTION('ref_axis',(0.,0.,-1.));
#1926=DIRECTION('center_axis',(1.,0.,0.));
#1927=DIRECTION('ref_axis',(0.,0.,-1.));
#1928=DIRECTION('',(1.,0.,0.));
#1929=DIRECTION('center_axis',(1.,0.,0.));
#1930=DIRECTION('ref_axis',(0.,0.,-1.));
#1931=DIRECTION('center_axis',(-1.,0.,0.));
#1932=DIRECTION('ref_axis',(0.,0.,1.));
#1933=DIRECTION('center_axis',(1.,0.,0.));
#1934=DIRECTION('ref_axis',(0.,0.,-1.));
#1935=DIRECTION('center_axis',(1.,0.,0.));
#1936=DIRECTION('ref_axis',(0.,0.,-1.));
#1937=DIRECTION('center_axis',(1.,0.,0.));
#1938=DIRECTION('ref_axis',(0.,0.,-1.));
#1939=DIRECTION('center_axis',(-1.,0.,0.));
#1940=DIRECTION('ref_axis',(0.,0.,1.));
#1941=DIRECTION('center_axis',(1.,0.,0.));
#1942=DIRECTION('ref_axis',(0.,0.,-1.));
#1943=DIRECTION('center_axis',(1.,0.,0.));
#1944=DIRECTION('ref_axis',(0.,0.,-1.));
#1945=DIRECTION('center_axis',(1.,0.,0.));
#1946=DIRECTION('ref_axis',(0.,0.,-1.));
#1947=DIRECTION('center_axis',(1.,0.,0.));
#1948=DIRECTION('ref_axis',(0.,0.,-1.));
#1949=DIRECTION('',(1.,0.,0.));
#1950=DIRECTION('center_axis',(-1.,0.,0.));
#1951=DIRECTION('ref_axis',(0.,0.,-1.));
#1952=DIRECTION('',(-0.704026902010687,8.69711463179084E-17,0.710173303669769));
#1953=DIRECTION('center_axis',(1.,0.,0.));
#1954=DIRECTION('ref_axis',(0.,0.,-1.));
#1955=DIRECTION('center_axis',(1.,0.,0.));
#1956=DIRECTION('ref_axis',(0.,0.,-1.));
#1957=DIRECTION('center_axis',(1.,0.,0.));
#1958=DIRECTION('ref_axis',(0.,0.,-1.));
#1959=DIRECTION('',(1.,0.,0.));
#1960=DIRECTION('center_axis',(-1.,0.,0.));
#1961=DIRECTION('ref_axis',(0.,0.,1.));
#1962=DIRECTION('center_axis',(1.,0.,0.));
#1963=DIRECTION('ref_axis',(0.,0.,-1.));
#1964=DIRECTION('center_axis',(1.,0.,0.));
#1965=DIRECTION('ref_axis',(0.,0.,-1.));
#1966=DIRECTION('center_axis',(1.,0.,0.));
#1967=DIRECTION('ref_axis',(0.,0.,-1.));
#1968=DIRECTION('',(-1.,0.,0.));
#1969=DIRECTION('',(-1.,0.,0.));
#1970=DIRECTION('center_axis',(1.,0.,0.));
#1971=DIRECTION('ref_axis',(0.,0.,-1.));
#1972=DIRECTION('center_axis',(1.,0.,0.));
#1973=DIRECTION('ref_axis',(0.,0.,-1.));
#1974=DIRECTION('center_axis',(1.,0.,0.));
#1975=DIRECTION('ref_axis',(0.,0.,-1.));
#1976=DIRECTION('center_axis',(1.,0.,0.));
#1977=DIRECTION('ref_axis',(0.,0.,-1.));
#1978=DIRECTION('',(1.,0.,0.));
#1979=DIRECTION('center_axis',(1.,0.,0.));
#1980=DIRECTION('ref_axis',(0.,0.,-1.));
#1981=DIRECTION('center_axis',(1.,0.,0.));
#1982=DIRECTION('ref_axis',(0.,0.,-1.));
#1983=DIRECTION('center_axis',(1.,0.,0.));
#1984=DIRECTION('ref_axis',(0.,0.,-1.));
#1985=DIRECTION('center_axis',(1.,0.,0.));
#1986=DIRECTION('ref_axis',(0.,0.,-1.));
#1987=DIRECTION('',(1.,0.,0.));
#1988=DIRECTION('center_axis',(1.,0.,0.));
#1989=DIRECTION('ref_axis',(0.,0.,-1.));
#1990=DIRECTION('axis',(0.,0.,1.));
#1991=DIRECTION('refdir',(1.,0.,0.));
#1992=DIRECTION('center_axis',(1.,0.,0.));
#1993=DIRECTION('ref_axis',(0.,0.,-1.));
#1994=DIRECTION('center_axis',(1.,0.,0.));
#1995=DIRECTION('ref_axis',(0.,0.,-1.));
#1996=DIRECTION('',(-1.,0.,0.));
#1997=DIRECTION('center_axis',(1.,0.,0.));
#1998=DIRECTION('ref_axis',(0.,0.,-1.));
#1999=DIRECTION('center_axis',(-1.,0.,0.));
#2000=DIRECTION('ref_axis',(0.,0.,-1.));
#2001=DIRECTION('',(0.707106781186548,-8.65956056235493E-17,-0.707106781186547));
#2002=DIRECTION('center_axis',(1.,0.,0.));
#2003=DIRECTION('ref_axis',(0.,0.,-1.));
#2004=DIRECTION('center_axis',(1.,0.,0.));
#2005=DIRECTION('ref_axis',(0.,0.,-1.));
#2006=DIRECTION('center_axis',(1.,0.,0.));
#2007=DIRECTION('ref_axis',(0.,0.,-1.));
#2008=DIRECTION('center_axis',(1.,0.,0.));
#2009=DIRECTION('ref_axis',(0.,0.,-1.));
#2010=DIRECTION('center_axis',(1.,0.,0.));
#2011=DIRECTION('ref_axis',(0.,0.,-1.));
#2012=DIRECTION('',(0.709323060095161,-8.63233363609118E-17,0.704883533938222));
#2013=DIRECTION('center_axis',(1.,0.,0.));
#2014=DIRECTION('ref_axis',(0.,0.,-1.));
#2015=DIRECTION('center_axis',(1.,0.,0.));
#2016=DIRECTION('ref_axis',(0.,0.,-1.));
#2017=DIRECTION('center_axis',(1.,0.,0.));
#2018=DIRECTION('ref_axis',(0.,0.,-1.));
#2019=DIRECTION('center_axis',(1.,0.,0.));
#2020=DIRECTION('ref_axis',(0.,0.,-1.));
#2021=DIRECTION('',(1.,0.,0.));
#2022=DIRECTION('center_axis',(-1.,0.,0.));
#2023=DIRECTION('ref_axis',(0.,0.,1.));
#2024=DIRECTION('center_axis',(1.,0.,0.));
#2025=DIRECTION('ref_axis',(0.,0.,-1.));
#2026=DIRECTION('center_axis',(1.,0.,0.));
#2027=DIRECTION('ref_axis',(0.,0.,-1.));
#2028=DIRECTION('center_axis',(1.,0.,0.));
#2029=DIRECTION('ref_axis',(0.,0.,-1.));
#2030=DIRECTION('',(1.,0.,0.));
#2031=DIRECTION('center_axis',(1.,0.,0.));
#2032=DIRECTION('ref_axis',(0.,0.,-1.));
#2033=DIRECTION('center_axis',(1.,0.,0.));
#2034=DIRECTION('ref_axis',(0.,0.,-1.));
#2035=DIRECTION('center_axis',(1.,0.,0.));
#2036=DIRECTION('ref_axis',(0.,0.,-1.));
#2037=DIRECTION('center_axis',(1.,0.,0.));
#2038=DIRECTION('ref_axis',(0.,0.,-1.));
#2039=DIRECTION('',(1.,0.,0.));
#2040=DIRECTION('center_axis',(-1.,0.,0.));
#2041=DIRECTION('ref_axis',(0.,0.,-1.));
#2042=DIRECTION('',(-0.703132298742306,8.70796187760308E-17,0.711059048508182));
#2043=DIRECTION('center_axis',(1.,0.,0.));
#2044=DIRECTION('ref_axis',(0.,0.,-1.));
#2045=DIRECTION('center_axis',(1.,0.,0.));
#2046=DIRECTION('ref_axis',(0.,0.,-1.));
#2047=DIRECTION('center_axis',(1.,0.,0.));
#2048=DIRECTION('ref_axis',(0.,0.,-1.));
#2049=DIRECTION('',(1.,0.,0.));
#2050=DIRECTION('center_axis',(-1.,0.,0.));
#2051=DIRECTION('ref_axis',(0.,0.,-1.));
#2052=DIRECTION('',(-0.703132298742305,8.70796187760308E-17,0.711059048508182));
#2053=DIRECTION('center_axis',(1.,0.,0.));
#2054=DIRECTION('ref_axis',(0.,0.,-1.));
#2055=DIRECTION('center_axis',(-1.,0.,0.));
#2056=DIRECTION('ref_axis',(0.,0.,1.));
#2057=DIRECTION('center_axis',(1.,0.,0.));
#2058=DIRECTION('ref_axis',(0.,0.,-1.));
#2059=DIRECTION('center_axis',(1.,0.,0.));
#2060=DIRECTION('ref_axis',(0.,0.,-1.));
#2061=DIRECTION('center_axis',(1.,0.,0.));
#2062=DIRECTION('ref_axis',(0.,0.,-1.));
#2063=DIRECTION('',(-0.711059048508181,8.61088719031886E-17,-0.703132298742306));
#2064=DIRECTION('center_axis',(1.,0.,0.));
#2065=DIRECTION('ref_axis',(0.,0.,-1.));
#2066=DIRECTION('center_axis',(1.,0.,0.));
#2067=DIRECTION('ref_axis',(0.,0.,-1.));
#2068=DIRECTION('',(-1.,0.,0.));
#2069=DIRECTION('center_axis',(-1.,0.,0.));
#2070=DIRECTION('ref_axis',(0.,0.,1.));
#2071=DIRECTION('center_axis',(1.,0.,0.));
#2072=DIRECTION('ref_axis',(0.,0.,-1.));
#2073=DIRECTION('center_axis',(1.,0.,0.));
#2074=DIRECTION('ref_axis',(0.,0.,-1.));
#2075=DIRECTION('',(-0.711059048508182,8.61088719031885E-17,-0.703132298742306));
#2076=DIRECTION('axis',(0.,0.,1.));
#2077=DIRECTION('refdir',(1.,0.,0.));
#2078=DIRECTION('center_axis',(-1.,0.,0.));
#2079=DIRECTION('ref_axis',(0.,0.,-1.));
#2080=DIRECTION('center_axis',(1.,0.,0.));
#2081=DIRECTION('ref_axis',(0.,0.,-1.));
#2082=DIRECTION('',(0.507743181153061,-1.05504360309624E-16,-0.861508480511115));
#2083=DIRECTION('center_axis',(1.,0.,0.));
#2084=DIRECTION('ref_axis',(0.,0.,-1.));
#2085=DIRECTION('center_axis',(1.,0.,0.));
#2086=DIRECTION('ref_axis',(0.,0.,-1.));
#2087=DIRECTION('center_axis',(1.,0.,0.));
#2088=DIRECTION('ref_axis',(0.,0.,-1.));
#2089=DIRECTION('',(-1.,0.,0.));
#2090=DIRECTION('center_axis',(-1.,0.,0.));
#2091=DIRECTION('ref_axis',(0.,0.,1.));
#2092=DIRECTION('center_axis',(1.,0.,0.));
#2093=DIRECTION('ref_axis',(0.,0.,-1.));
#2094=DIRECTION('center_axis',(1.,0.,0.));
#2095=DIRECTION('ref_axis',(0.,0.,-1.));
#2096=DIRECTION('center_axis',(1.,0.,0.));
#2097=DIRECTION('ref_axis',(0.,0.,-1.));
#2098=DIRECTION('',(-0.472810273503224,1.07911498508989E-16,-0.88116425555614));
#2099=DIRECTION('center_axis',(1.,0.,0.));
#2100=DIRECTION('ref_axis',(0.,0.,-1.));
#2101=DIRECTION('center_axis',(1.,0.,0.));
#2102=DIRECTION('ref_axis',(0.,0.,-1.));
#2103=DIRECTION('',(-1.,0.,0.));
#2104=DIRECTION('center_axis',(-1.,0.,0.));
#2105=DIRECTION('ref_axis',(0.,0.,-1.));
#2106=DIRECTION('',(0.504883315037955,-1.0570999352361E-16,-0.863187603129404));
#2107=DIRECTION('center_axis',(1.,0.,0.));
#2108=DIRECTION('ref_axis',(0.,0.,-1.));
#2109=DIRECTION('center_axis',(1.,0.,0.));
#2110=DIRECTION('ref_axis',(0.,0.,-1.));
#2111=DIRECTION('center_axis',(1.,0.,0.));
#2112=DIRECTION('ref_axis',(0.,0.,-1.));
#2113=DIRECTION('center_axis',(1.,0.,0.));
#2114=DIRECTION('ref_axis',(0.,0.,-1.));
#2115=DIRECTION('center_axis',(1.,0.,0.));
#2116=DIRECTION('ref_axis',(0.,0.,-1.));
#2117=DIRECTION('',(1.,0.,0.));
#2118=DIRECTION('center_axis',(1.,0.,0.));
#2119=DIRECTION('ref_axis',(0.,0.,-1.));
#2120=DIRECTION('center_axis',(-1.,0.,0.));
#2121=DIRECTION('ref_axis',(0.,0.,1.));
#2122=DIRECTION('center_axis',(1.,0.,0.));
#2123=DIRECTION('ref_axis',(0.,0.,-1.));
#2124=DIRECTION('center_axis',(1.,0.,0.));
#2125=DIRECTION('ref_axis',(0.,0.,-1.));
#2126=DIRECTION('center_axis',(1.,0.,0.));
#2127=DIRECTION('ref_axis',(0.,0.,-1.));
#2128=DIRECTION('',(-1.,0.,0.));
#2129=DIRECTION('center_axis',(-1.,0.,0.));
#2130=DIRECTION('ref_axis',(0.,0.,1.));
#2131=DIRECTION('center_axis',(1.,0.,0.));
#2132=DIRECTION('ref_axis',(0.,0.,-1.));
#2133=DIRECTION('center_axis',(1.,0.,0.));
#2134=DIRECTION('ref_axis',(0.,0.,-1.));
#2135=DIRECTION('',(-1.,0.,0.));
#2136=DIRECTION('axis',(0.,0.,1.));
#2137=DIRECTION('refdir',(1.,0.,0.));
#2138=DIRECTION('center_axis',(1.,0.,0.));
#2139=DIRECTION('ref_axis',(0.,0.,-1.));
#2140=DIRECTION('center_axis',(1.,0.,0.));
#2141=DIRECTION('ref_axis',(0.,0.,-1.));
#2142=DIRECTION('',(-0.67994690492187,8.97986164450499E-17,-0.733261349374948));
#2143=DIRECTION('center_axis',(1.,0.,0.));
#2144=DIRECTION('ref_axis',(0.,0.,-1.));
#2145=DIRECTION('center_axis',(1.,0.,0.));
#2146=DIRECTION('ref_axis',(0.,0.,-1.));
#2147=DIRECTION('center_axis',(1.,0.,0.));
#2148=DIRECTION('ref_axis',(0.,0.,-1.));
#2149=DIRECTION('',(-1.,0.,0.));
#2150=DIRECTION('center_axis',(1.,0.,0.));
#2151=DIRECTION('ref_axis',(0.,0.,-1.));
#2152=DIRECTION('center_axis',(1.,0.,0.));
#2153=DIRECTION('ref_axis',(0.,0.,-1.));
#2154=DIRECTION('center_axis',(1.,0.,0.));
#2155=DIRECTION('ref_axis',(0.,0.,-1.));
#2156=DIRECTION('center_axis',(1.,0.,0.));
#2157=DIRECTION('ref_axis',(0.,0.,-1.));
#2158=DIRECTION('',(-1.,0.,0.));
#2159=DIRECTION('center_axis',(-1.,0.,0.));
#2160=DIRECTION('ref_axis',(0.,0.,1.));
#2161=DIRECTION('center_axis',(1.,0.,0.));
#2162=DIRECTION('ref_axis',(0.,0.,-1.));
#2163=DIRECTION('center_axis',(1.,0.,0.));
#2164=DIRECTION('ref_axis',(0.,0.,-1.));
#2165=DIRECTION('center_axis',(1.,0.,0.));
#2166=DIRECTION('ref_axis',(0.,0.,-1.));
#2167=DIRECTION('',(-1.,0.,0.));
#2168=DIRECTION('center_axis',(1.,0.,0.));
#2169=DIRECTION('ref_axis',(0.,0.,-1.));
#2170=DIRECTION('center_axis',(1.,0.,0.));
#2171=DIRECTION('ref_axis',(0.,0.,-1.));
#2172=DIRECTION('center_axis',(1.,0.,0.));
#2173=DIRECTION('ref_axis',(0.,0.,-1.));
#2174=DIRECTION('center_axis',(1.,0.,0.));
#2175=DIRECTION('ref_axis',(0.,0.,-1.));
#2176=DIRECTION('',(0.0135953438732625,-1.22453361611656E-16,0.999907579041667));
#2177=DIRECTION('center_axis',(1.,0.,0.));
#2178=DIRECTION('ref_axis',(0.,0.,-1.));
#2179=DIRECTION('center_axis',(1.,0.,0.));
#2180=DIRECTION('ref_axis',(0.,0.,-1.));
#2181=DIRECTION('',(1.,0.,0.));
#2182=DIRECTION('center_axis',(-1.,0.,0.));
#2183=DIRECTION('ref_axis',(0.,0.,1.));
#2184=DIRECTION('axis',(0.,0.,1.));
#2185=DIRECTION('refdir',(1.,0.,0.));
#2186=DIRECTION('',(0.,0.769537968693233,-0.638601060709652));
#2187=DIRECTION('center_axis',(1.,0.,0.));
#2188=DIRECTION('ref_axis',(0.,0.,-1.));
#2189=DIRECTION('center_axis',(1.,0.,0.));
#2190=DIRECTION('ref_axis',(0.,0.,-1.));
#2191=DIRECTION('',(-1.,0.,0.));
#2192=DIRECTION('',(-1.,0.,0.));
#2193=DIRECTION('center_axis',(1.,0.,0.));
#2194=DIRECTION('ref_axis',(0.,0.,-1.));
#2195=DIRECTION('center_axis',(0.,1.83697019872103E-16,1.));
#2196=DIRECTION('ref_axis',(1.,0.,0.));
#2197=DIRECTION('center_axis',(0.,1.83697019872103E-16,1.));
#2198=DIRECTION('ref_axis',(1.,0.,0.));
#2199=DIRECTION('',(0.,1.83697019872103E-16,1.));
#2200=DIRECTION('',(0.,-0.63860106070965,-0.769537968693234));
#2201=DIRECTION('center_axis',(0.,1.,-1.22464679914735E-16));
#2202=DIRECTION('ref_axis',(1.,0.,0.));
#2203=DIRECTION('center_axis',(0.,1.,-1.22464679914735E-16));
#2204=DIRECTION('ref_axis',(1.,0.,0.));
#2205=DIRECTION('',(0.,1.,-1.22464679914735E-16));
#2206=DIRECTION('',(0.,-0.769537968693233,0.638601060709652));
#2207=DIRECTION('center_axis',(0.,-6.12323399573677E-17,-1.));
#2208=DIRECTION('ref_axis',(1.,0.,0.));
#2209=DIRECTION('center_axis',(0.,-6.12323399573677E-17,-1.));
#2210=DIRECTION('ref_axis',(1.,0.,0.));
#2211=DIRECTION('',(0.,-6.12323399573677E-17,-1.));
#2212=DIRECTION('center_axis',(0.,-1.83697019872103E-16,-1.));
#2213=DIRECTION('ref_axis',(1.,0.,0.));
#2214=DIRECTION('center_axis',(0.,-1.,1.22464679914735E-16));
#2215=DIRECTION('ref_axis',(1.,0.,0.));
#2216=DIRECTION('center_axis',(0.,6.12323399573677E-17,1.));
#2217=DIRECTION('ref_axis',(1.,0.,0.));
#2218=DIRECTION('',(0.,0.638601060709651,0.769537968693234));
#2219=DIRECTION('center_axis',(0.,-1.,0.));
#2220=DIRECTION('ref_axis',(1.,0.,0.));
#2221=DIRECTION('center_axis',(0.,-1.,0.));
#2222=DIRECTION('ref_axis',(1.,0.,0.));
#2223=DIRECTION('',(0.,-1.,0.));
#2224=DIRECTION('center_axis',(0.,1.,0.));
#2225=DIRECTION('ref_axis',(1.,0.,0.));
#2226=DIRECTION('center_axis',(-1.,0.,0.));
#2227=DIRECTION('ref_axis',(0.,0.,1.));
#2228=DIRECTION('center_axis',(1.,0.,0.));
#2229=DIRECTION('ref_axis',(0.,0.,-1.));
#2230=DIRECTION('center_axis',(1.,0.,0.));
#2231=DIRECTION('ref_axis',(0.,0.,-1.));
#2232=DIRECTION('center_axis',(1.,0.,0.));
#2233=DIRECTION('ref_axis',(0.,0.,-1.));
#2234=DIRECTION('',(-0.681644128816632,8.9605430606225E-17,-0.731683867288199));
#2235=DIRECTION('center_axis',(-1.,0.,0.));
#2236=DIRECTION('ref_axis',(0.,0.,-1.));
#2237=DIRECTION('',(0.681644128816632,-8.9605430606225E-17,-0.731683867288199));
#2238=DIRECTION('center_axis',(1.,0.,0.));
#2239=DIRECTION('ref_axis',(0.,0.,-1.));
#2240=DIRECTION('center_axis',(1.,0.,0.));
#2241=DIRECTION('ref_axis',(0.,0.,-1.));
#2242=DIRECTION('center_axis',(1.,0.,0.));
#2243=DIRECTION('ref_axis',(0.,0.,-1.));
#2244=DIRECTION('center_axis',(1.,0.,0.));
#2245=DIRECTION('ref_axis',(0.,0.,-1.));
#2246=DIRECTION('center_axis',(1.,0.,0.));
#2247=DIRECTION('ref_axis',(0.,0.,-1.));
#2248=DIRECTION('',(0.501761337735621,-1.05932695650405E-16,0.865006103997978));
#2249=DIRECTION('center_axis',(1.,0.,0.));
#2250=DIRECTION('ref_axis',(0.,0.,-1.));
#2251=DIRECTION('center_axis',(1.,0.,0.));
#2252=DIRECTION('ref_axis',(0.,0.,-1.));
#2253=DIRECTION('',(1.,0.,0.));
#2254=DIRECTION('center_axis',(-1.,0.,0.));
#2255=DIRECTION('ref_axis',(0.,0.,-1.));
#2256=DIRECTION('',(-0.501761337735621,1.05932695650405E-16,0.865006103997978));
#2257=DIRECTION('axis',(0.,0.,1.));
#2258=DIRECTION('refdir',(1.,0.,0.));
#2259=DIRECTION('center_axis',(1.57016756309984E-16,-1.,0.));
#2260=DIRECTION('ref_axis',(1.,1.57016756309984E-16,0.));
#2261=DIRECTION('',(1.,0.,0.));
#2262=DIRECTION('',(0.,0.,-1.));
#2263=DIRECTION('',(-1.,0.,0.));
#2264=DIRECTION('',(0.,0.,-1.));
#2265=DIRECTION('center_axis',(1.57016756309984E-16,-1.,0.));
#2266=DIRECTION('ref_axis',(1.,1.57016756309984E-16,0.));
#2267=DIRECTION('',(-1.,0.,0.));
#2268=DIRECTION('',(0.,0.,-1.));
#2269=DIRECTION('',(1.,0.,0.));
#2270=DIRECTION('',(0.,0.,-1.));
#2271=DIRECTION('center_axis',(0.,0.,1.));
#2272=DIRECTION('ref_axis',(-6.34413156928666E-15,-1.,0.));
#2273=DIRECTION('',(0.,0.,1.));
#2274=DIRECTION('center_axis',(1.,0.,0.));
#2275=DIRECTION('ref_axis',(0.,1.,0.));
#2276=DIRECTION('center_axis',(1.,0.,0.));
#2277=DIRECTION('ref_axis',(0.,0.,-1.));
#2278=DIRECTION('center_axis',(-1.,0.,0.));
#2279=DIRECTION('ref_axis',(0.,0.,-1.));
#2280=DIRECTION('',(0.,0.,1.));
#2281=DIRECTION('center_axis',(-2.35525134464976E-16,1.,0.));
#2282=DIRECTION('ref_axis',(-1.,-2.35525134464976E-16,0.));
#2283=DIRECTION('',(-1.,0.,0.));
#2284=DIRECTION('',(0.,0.,1.));
#2285=DIRECTION('',(1.,0.,0.));
#2286=DIRECTION('',(0.,0.,1.));
#2287=DIRECTION('center_axis',(0.,0.,1.));
#2288=DIRECTION('ref_axis',(1.,1.11517937741366E-16,0.));
#2289=DIRECTION('center_axis',(-2.35525134464976E-16,1.,0.));
#2290=DIRECTION('ref_axis',(-1.,-2.35525134464976E-16,0.));
#2291=DIRECTION('',(1.,0.,0.));
#2292=DIRECTION('',(0.,0.,1.));
#2293=DIRECTION('',(-1.,0.,0.));
#2294=DIRECTION('',(0.,0.,1.));
#2295=DIRECTION('center_axis',(0.,0.,1.));
#2296=DIRECTION('ref_axis',(1.,1.11517937741366E-16,0.));
#2297=DIRECTION('',(0.,0.,1.));
#2298=DIRECTION('center_axis',(1.,0.,0.));
#2299=DIRECTION('ref_axis',(0.,1.,0.));
#2300=DIRECTION('center_axis',(1.,0.,0.));
#2301=DIRECTION('ref_axis',(0.,0.,-1.));
#2302=DIRECTION('center_axis',(-1.,0.,0.));
#2303=DIRECTION('ref_axis',(0.,0.,-1.));
#2304=DIRECTION('center_axis',(-1.,0.,0.));
#2305=DIRECTION('ref_axis',(0.,0.,-1.));
#2306=DIRECTION('',(0.,0.,1.));
#2307=DIRECTION('center_axis',(1.,0.,0.));
#2308=DIRECTION('ref_axis',(0.,0.,-1.));
#2309=DIRECTION('center_axis',(0.,0.,1.));
#2310=DIRECTION('ref_axis',(-6.34413156928666E-15,-1.,0.));
#2311=DIRECTION('center_axis',(1.,0.,0.));
#2312=DIRECTION('ref_axis',(0.,0.,-1.));
#2313=DIRECTION('center_axis',(1.,0.,0.));
#2314=DIRECTION('ref_axis',(0.,0.,-1.));
#2315=DIRECTION('center_axis',(0.,1.,1.22464679914735E-16));
#2316=DIRECTION('ref_axis',(0.,-1.22464679914735E-16,1.));
#2317=DIRECTION('center_axis',(1.,0.,0.));
#2318=DIRECTION('ref_axis',(0.,0.,-1.));
#2319=DIRECTION('center_axis',(1.,0.,0.));
#2320=DIRECTION('ref_axis',(0.,0.,-1.));
#2321=DIRECTION('center_axis',(1.,0.,0.));
#2322=DIRECTION('ref_axis',(0.,0.,-1.));
#2323=DIRECTION('',(1.,0.,0.));
#2324=DIRECTION('center_axis',(1.,0.,0.));
#2325=DIRECTION('ref_axis',(0.,0.,-1.));
#2326=DIRECTION('center_axis',(1.,0.,0.));
#2327=DIRECTION('ref_axis',(0.,0.,-1.));
#2328=DIRECTION('center_axis',(1.,0.,0.));
#2329=DIRECTION('ref_axis',(0.,0.,-1.));
#2330=DIRECTION('center_axis',(1.,0.,0.));
#2331=DIRECTION('ref_axis',(0.,0.,-1.));
#2332=DIRECTION('center_axis',(1.,0.,0.));
#2333=DIRECTION('ref_axis',(0.,0.,-1.));
#2334=DIRECTION('center_axis',(1.,0.,0.));
#2335=DIRECTION('ref_axis',(0.,0.,-1.));
#2336=DIRECTION('center_axis',(1.,0.,0.));
#2337=DIRECTION('ref_axis',(0.,0.,-1.));
#2338=DIRECTION('center_axis',(-1.,0.,0.));
#2339=DIRECTION('ref_axis',(0.,0.,1.));
#2340=DIRECTION('center_axis',(-1.,0.,0.));
#2341=DIRECTION('ref_axis',(0.,0.,1.));
#2342=DIRECTION('center_axis',(1.,0.,0.));
#2343=DIRECTION('ref_axis',(0.,0.,-1.));
#2344=DIRECTION('center_axis',(1.,0.,0.));
#2345=DIRECTION('ref_axis',(0.,0.,-1.));
#2346=DIRECTION('center_axis',(1.,0.,0.));
#2347=DIRECTION('ref_axis',(0.,0.,-1.));
#2348=DIRECTION('center_axis',(1.,0.,0.));
#2349=DIRECTION('ref_axis',(0.,0.,-1.));
#2350=DIRECTION('',(-1.,0.,0.));
#2351=DIRECTION('center_axis',(1.,0.,0.));
#2352=DIRECTION('ref_axis',(0.,0.,-1.));
#2353=DIRECTION('center_axis',(1.,0.,0.));
#2354=DIRECTION('ref_axis',(0.,0.,-1.));
#2355=DIRECTION('',(-0.513577720619322,1.05079970984514E-16,-0.858043078687464));
#2356=DIRECTION('center_axis',(1.,0.,0.));
#2357=DIRECTION('ref_axis',(0.,0.,-1.));
#2358=DIRECTION('center_axis',(1.,0.,0.));
#2359=DIRECTION('ref_axis',(0.,0.,-1.));
#2360=DIRECTION('',(-1.,0.,0.));
#2361=DIRECTION('center_axis',(-1.,0.,0.));
#2362=DIRECTION('ref_axis',(0.,0.,-1.));
#2363=DIRECTION('',(0.983571141526098,-2.21074390598966E-17,-0.180520939386676));
#2364=DIRECTION('center_axis',(1.,0.,0.));
#2365=DIRECTION('ref_axis',(0.,0.,-1.));
#2366=DIRECTION('center_axis',(1.,0.,0.));
#2367=DIRECTION('ref_axis',(0.,0.,-1.));
#2368=DIRECTION('center_axis',(1.,0.,0.));
#2369=DIRECTION('ref_axis',(0.,0.,-1.));
#2370=DIRECTION('center_axis',(1.,0.,0.));
#2371=DIRECTION('ref_axis',(0.,0.,-1.));
#2372=DIRECTION('',(1.,0.,0.));
#2373=DIRECTION('axis',(0.,0.,1.));
#2374=DIRECTION('refdir',(1.,0.,0.));
#2375=DIRECTION('center_axis',(0.,0.,-1.));
#2376=DIRECTION('ref_axis',(1.,0.,0.));
#2377=DIRECTION('center_axis',(0.,0.,1.));
#2378=DIRECTION('ref_axis',(1.,0.,0.));
#2379=DIRECTION('',(0.707106781186539,-8.65956056235483E-17,0.707106781186556));
#2380=DIRECTION('center_axis',(0.,0.,-1.));
#2381=DIRECTION('ref_axis',(1.,0.,0.));
#2382=DIRECTION('center_axis',(0.,0.,1.));
#2383=DIRECTION('ref_axis',(1.,0.,0.));
#2384=DIRECTION('',(0.,0.,-1.));
#2385=DIRECTION('center_axis',(0.,0.,1.));
#2386=DIRECTION('ref_axis',(1.,0.,0.));
#2387=DIRECTION('center_axis',(0.,0.,1.));
#2388=DIRECTION('ref_axis',(1.,0.,0.));
#2389=DIRECTION('center_axis',(0.,0.,1.));
#2390=DIRECTION('ref_axis',(1.,0.,0.));
#2391=DIRECTION('',(0.,0.,1.));
#2392=DIRECTION('',(1.,0.,0.));
#2393=DIRECTION('',(0.,0.,1.));
#2394=DIRECTION('',(1.,0.,0.));
#2395=DIRECTION('',(0.,0.,1.));
#2396=DIRECTION('',(1.,0.,0.));
#2397=DIRECTION('',(0.,0.,1.));
#2398=DIRECTION('',(1.,0.,0.));
#2399=DIRECTION('',(0.,0.,1.));
#2400=DIRECTION('',(1.,0.,0.));
#2401=DIRECTION('',(0.,0.,1.));
#2402=DIRECTION('',(1.,0.,0.));
#2403=DIRECTION('',(0.,0.,1.));
#2404=DIRECTION('',(1.,0.,0.));
#2405=DIRECTION('',(0.,0.,1.));
#2406=DIRECTION('',(1.,0.,0.));
#2407=CARTESIAN_POINT('',(0.,0.,0.));
#2408=CARTESIAN_POINT('',(0.,0.,0.));
#2409=CARTESIAN_POINT('Origin',(-28.33623852117,0.,0.));
#2410=CARTESIAN_POINT('',(-26.5531819279316,1.09180727480402E-16,2.67415656874908E-32));
#2411=CARTESIAN_POINT('',(-30.1192951144084,1.09180727480402E-16,-6.84227765783602E-48));
#2412=CARTESIAN_POINT('Origin',(-28.33623852117,0.,0.));
#2413=CARTESIAN_POINT('',(0.,0.,0.));
#2414=CARTESIAN_POINT('Origin',(-25.2637346688979,0.,1.77272245287895));
#2415=CARTESIAN_POINT('',(-24.6656713617233,0.0481692911654238,-0.227277547121048));
#2416=CARTESIAN_POINT('',(-24.6656713617233,0.0481692911654247,0.897611603555783));
#2417=CARTESIAN_POINT('',(-24.6656713617233,0.0481692911654238,1.77272245287895));
#2418=CARTESIAN_POINT('',(-24.6656713617233,-0.0481692911654238,-0.227277547121048));
#2419=CARTESIAN_POINT('Origin',(-25.2637346688979,0.,-0.227277547121048));
#2420=CARTESIAN_POINT('',(-24.6656713617233,-0.0481692911654247,0.897611603555783));
#2421=CARTESIAN_POINT('',(-24.6656713617233,-0.0481692911654238,1.77272245287895));
#2422=CARTESIAN_POINT('',(-24.7560377201621,-0.319755857247933,0.840108959126733));
#2423=CARTESIAN_POINT('Ctrl Pts',(-24.7560377201621,-0.319755857247933,
0.840108959126733));
#2424=CARTESIAN_POINT('Ctrl Pts',(-24.7389020605853,-0.292548467970954,
0.850464427887334));
#2425=CARTESIAN_POINT('Ctrl Pts',(-24.7237010096035,-0.263521886093109,
0.859980342899897));
#2426=CARTESIAN_POINT('Ctrl Pts',(-24.686207592206,-0.174658036922562,0.883855860882441));
#2427=CARTESIAN_POINT('Ctrl Pts',(-24.6707368006861,-0.111061086022905,
0.894236587940559));
#2428=CARTESIAN_POINT('Ctrl Pts',(-24.6656713617233,-0.0481692911654243,
0.897611603555783));
#2429=CARTESIAN_POINT('',(-24.7560377201621,-0.319755857247933,1.15456014751321));
#2430=CARTESIAN_POINT('',(-24.7560377201621,-0.319755857247933,1.77272245287895));
#2431=CARTESIAN_POINT('',(-25.8637346688979,-6.49286604591722E-17,1.19802042656629));
#2432=CARTESIAN_POINT('Ctrl Pts',(-25.8637346688979,-5.63785129692462E-17,
1.19802042656629));
#2433=CARTESIAN_POINT('Ctrl Pts',(-25.8637346688979,-0.0767782567949871,
1.19802042656629));
#2434=CARTESIAN_POINT('Ctrl Pts',(-25.8481109979872,-0.157774416814917,
1.18996152111882));
#2435=CARTESIAN_POINT('Ctrl Pts',(-25.7864300204004,-0.30525073804353,1.16091479971318));
#2436=CARTESIAN_POINT('Ctrl Pts',(-25.7404416616373,-0.371821144684504,
1.14023972009026));
#2437=CARTESIAN_POINT('Ctrl Pts',(-25.6354113717621,-0.476851434559632,
1.10046700926426));
#2438=CARTESIAN_POINT('Ctrl Pts',(-25.5688895915929,-0.522733853172129,
1.07852127007884));
#2439=CARTESIAN_POINT('Ctrl Pts',(-25.4216260093517,-0.584328998785629,
1.04643134391016));
#2440=CARTESIAN_POINT('Ctrl Pts',(-25.3407243935196,-0.600000000000001,
1.03694404018253));
#2441=CARTESIAN_POINT('Ctrl Pts',(-25.2637346688979,-0.600000000000001,
1.03694404018253));
#2442=CARTESIAN_POINT('Ctrl Pts',(-25.1867449442762,-0.600000000000001,
1.03694404018253));
#2443=CARTESIAN_POINT('Ctrl Pts',(-25.1058433284441,-0.584328998785631,
1.04643134391016));
#2444=CARTESIAN_POINT('Ctrl Pts',(-24.9585797462029,-0.522733853172133,
1.07852127007884));
#2445=CARTESIAN_POINT('Ctrl Pts',(-24.8920579660337,-0.476851434559632,
1.10046700926426));
#2446=CARTESIAN_POINT('Ctrl Pts',(-24.8089379020593,-0.393731370585291,
1.13194278898667));
#2447=CARTESIAN_POINT('Ctrl Pts',(-24.7804480917521,-0.358513774867966,
1.14382612798167));
#2448=CARTESIAN_POINT('Ctrl Pts',(-24.7560377201621,-0.319755857247933,
1.15456014751321));
#2449=CARTESIAN_POINT('',(-25.8637346688979,-7.34788079488413E-17,1.9840612380693));
#2450=CARTESIAN_POINT('',(-25.8637346688979,-7.34788079488413E-17,1.77272245287895));
#2451=CARTESIAN_POINT('',(-25.2637346688979,-0.600000000000001,1.89116339759659));
#2452=CARTESIAN_POINT('Ctrl Pts',(-25.2637346688979,-0.600000000000001,
1.89116339759659));
#2453=CARTESIAN_POINT('Ctrl Pts',(-25.339599070486,-0.600000000000001,1.89116339759659));
#2454=CARTESIAN_POINT('Ctrl Pts',(-25.4201684023226,-0.584740786326485,
1.89620635355867));
#2455=CARTESIAN_POINT('Ctrl Pts',(-25.5678391532475,-0.523367759786817,
1.91405498074209));
#2456=CARTESIAN_POINT('Ctrl Pts',(-25.6349858006078,-0.477277005713967,
1.926564479109));
#2457=CARTESIAN_POINT('Ctrl Pts',(-25.7409953444987,-0.371267461823086,
1.94976990694802));
#2458=CARTESIAN_POINT('Ctrl Pts',(-25.7870987390016,-0.3041141877551,1.9620248365967));
#2459=CARTESIAN_POINT('Ctrl Pts',(-25.8484811044704,-0.156419315054409,
1.97928267214026));
#2460=CARTESIAN_POINT('Ctrl Pts',(-25.8637346688979,-0.0758410323063,1.9840612380693));
#2461=CARTESIAN_POINT('Ctrl Pts',(-25.8637346688979,8.23993651088983E-17,
1.9840612380693));
#2462=CARTESIAN_POINT('',(-24.6637346688979,-1.12815094845811E-16,1.9840612380693));
#2463=CARTESIAN_POINT('Ctrl Pts',(-24.6637346688979,1.73472347600281E-17,
1.9840612380693));
#2464=CARTESIAN_POINT('Ctrl Pts',(-24.6637346688979,-0.0758410323063,1.9840612380693));
#2465=CARTESIAN_POINT('Ctrl Pts',(-24.6789882333254,-0.156419315054409,
1.97928267214026));
#2466=CARTESIAN_POINT('Ctrl Pts',(-24.7403705987942,-0.304114187755101,
1.9620248365967));
#2467=CARTESIAN_POINT('Ctrl Pts',(-24.7864739932971,-0.371267461823086,
1.94976990694802));
#2468=CARTESIAN_POINT('Ctrl Pts',(-24.892483537188,-0.477277005713967,1.926564479109));
#2469=CARTESIAN_POINT('Ctrl Pts',(-24.9596301845483,-0.523367759786817,
1.91405498074209));
#2470=CARTESIAN_POINT('Ctrl Pts',(-25.1073009354732,-0.584740786326485,
1.89620635355867));
#2471=CARTESIAN_POINT('Ctrl Pts',(-25.1878702673098,-0.600000000000001,
1.89116339759659));
#2472=CARTESIAN_POINT('Ctrl Pts',(-25.2637346688979,-0.600000000000001,
1.89116339759659));
#2473=CARTESIAN_POINT('Ctrl Pts',(-25.8637346688979,8.23993651088983E-17,
1.9840612380693));
#2474=CARTESIAN_POINT('Ctrl Pts',(-25.8637346688979,0.0758410323063001,
1.9840612380693));
#2475=CARTESIAN_POINT('Ctrl Pts',(-25.8484811044704,0.156419315054409,1.97928267214026));
#2476=CARTESIAN_POINT('Ctrl Pts',(-25.7870987390016,0.304114187755101,1.9620248365967));
#2477=CARTESIAN_POINT('Ctrl Pts',(-25.7409953444987,0.371267461823086,1.94976990694802));
#2478=CARTESIAN_POINT('Ctrl Pts',(-25.6349858006078,0.477277005713967,1.926564479109));
#2479=CARTESIAN_POINT('Ctrl Pts',(-25.5678391532475,0.523367759786817,1.91405498074209));
#2480=CARTESIAN_POINT('Ctrl Pts',(-25.4201684023226,0.584740786326485,1.89620635355867));
#2481=CARTESIAN_POINT('Ctrl Pts',(-25.339599070486,0.600000000000001,1.89116339759659));
#2482=CARTESIAN_POINT('Ctrl Pts',(-25.1878702673098,0.600000000000001,1.89116339759659));
#2483=CARTESIAN_POINT('Ctrl Pts',(-25.1073009354732,0.584740786326485,1.89620635355867));
#2484=CARTESIAN_POINT('Ctrl Pts',(-24.9596301845483,0.523367759786817,1.91405498074209));
#2485=CARTESIAN_POINT('Ctrl Pts',(-24.892483537188,0.477277005713967,1.926564479109));
#2486=CARTESIAN_POINT('Ctrl Pts',(-24.7864739932971,0.371267461823086,1.94976990694802));
#2487=CARTESIAN_POINT('Ctrl Pts',(-24.7403705987942,0.304114187755098,1.9620248365967));
#2488=CARTESIAN_POINT('Ctrl Pts',(-24.6789882333254,0.156419315054404,1.97928267214026));
#2489=CARTESIAN_POINT('Ctrl Pts',(-24.6637346688979,0.0758410323063001,
1.9840612380693));
#2490=CARTESIAN_POINT('Ctrl Pts',(-24.6637346688979,1.73472347597681E-17,
1.9840612380693));
#2491=CARTESIAN_POINT('',(-24.7560377201621,0.319755857247933,1.15456014751321));
#2492=CARTESIAN_POINT('Ctrl Pts',(-24.7560377201621,0.319755857247933,1.15456014751321));
#2493=CARTESIAN_POINT('Ctrl Pts',(-24.7804480917171,0.358513774812489,1.14382612799704));
#2494=CARTESIAN_POINT('Ctrl Pts',(-24.8089379021649,0.393731370690889,1.13194278894668));
#2495=CARTESIAN_POINT('Ctrl Pts',(-24.8920579660337,0.476851434559632,1.10046700926426));
#2496=CARTESIAN_POINT('Ctrl Pts',(-24.9585797462029,0.522733853172133,1.07852127007884));
#2497=CARTESIAN_POINT('Ctrl Pts',(-25.1058433284441,0.584328998785631,1.04643134391016));
#2498=CARTESIAN_POINT('Ctrl Pts',(-25.1867449442762,0.600000000000001,1.03694404018253));
#2499=CARTESIAN_POINT('Ctrl Pts',(-25.3407243935196,0.600000000000001,1.03694404018253));
#2500=CARTESIAN_POINT('Ctrl Pts',(-25.4216260093517,0.584328998785631,1.04643134391016));
#2501=CARTESIAN_POINT('Ctrl Pts',(-25.5688895915929,0.522733853172133,1.07852127007884));
#2502=CARTESIAN_POINT('Ctrl Pts',(-25.6354113717621,0.476851434559632,1.10046700926426));
#2503=CARTESIAN_POINT('Ctrl Pts',(-25.7404416616373,0.371821144684504,1.14023972009026));
#2504=CARTESIAN_POINT('Ctrl Pts',(-25.7864300204004,0.305250738043532,1.16091479971318));
#2505=CARTESIAN_POINT('Ctrl Pts',(-25.8481109979872,0.157774416814918,1.18996152111882));
#2506=CARTESIAN_POINT('Ctrl Pts',(-25.8637346688979,0.076778256794987,1.19802042656629));
#2507=CARTESIAN_POINT('Ctrl Pts',(-25.8637346688979,-5.63785129695031E-17,
1.19802042656629));
#2508=CARTESIAN_POINT('',(-24.7560377201621,0.319755857247933,0.840108959126733));
#2509=CARTESIAN_POINT('',(-24.7560377201621,0.319755857247933,1.77272245287895));
#2510=CARTESIAN_POINT('Ctrl Pts',(-24.6656713617233,0.0481692911654243,
0.897611603555783));
#2511=CARTESIAN_POINT('Ctrl Pts',(-24.6707368006861,0.111061086022906,0.894236587940559));
#2512=CARTESIAN_POINT('Ctrl Pts',(-24.686207592206,0.174658036922562,0.883855860882441));
#2513=CARTESIAN_POINT('Ctrl Pts',(-24.7237010096035,0.263521886093109,0.859980342899897));
#2514=CARTESIAN_POINT('Ctrl Pts',(-24.7389020605853,0.292548467970953,0.850464427887335));
#2515=CARTESIAN_POINT('Ctrl Pts',(-24.7560377201621,0.319755857247933,0.840108959126733));
#2516=CARTESIAN_POINT('Origin',(-25.2637346688979,0.,-0.227277547121048));
#2517=CARTESIAN_POINT('',(-24.6656713617233,0.,-0.227277547121048));
#2518=CARTESIAN_POINT('Origin',(-25.5549741096415,0.,0.));
#2519=CARTESIAN_POINT('',(-26.3539104991209,-1.46715188070755E-16,1.19802042656629));
#2520=CARTESIAN_POINT('Origin',(-26.3539104991209,0.,0.));
#2521=CARTESIAN_POINT('',(-25.5549741096415,-1.46715188070755E-16,1.19802042656629));
#2522=CARTESIAN_POINT('Origin',(-24.7560377201621,0.,0.));
#2523=CARTESIAN_POINT('Origin',(-24.6656713617233,0.,-0.898903149093028));
#2524=CARTESIAN_POINT('Origin',(-24.6656713617233,0.,0.));
#2525=CARTESIAN_POINT('Origin',(-24.7108545409427,0.,0.));
#2526=CARTESIAN_POINT('Origin',(-24.7560377201621,0.,0.));
#2527=CARTESIAN_POINT('Origin',(-24.7560377201621,0.,-1.19802042656629));
#2528=CARTESIAN_POINT('Origin',(-26.3539104991209,0.,-0.898903149093028));
#2529=CARTESIAN_POINT('',(-26.3539104991209,-1.10083886428025E-16,0.898903149093028));
#2530=CARTESIAN_POINT('Origin',(-26.3539104991209,0.,0.));
#2531=CARTESIAN_POINT('Origin',(-26.5296283843145,0.,0.));
#2532=CARTESIAN_POINT('',(-26.7053462695082,-1.10083886428025E-16,0.898903149093028));
#2533=CARTESIAN_POINT('Origin',(-26.7053462695082,0.,0.));
#2534=CARTESIAN_POINT('',(-26.5296283843145,-1.10083886428025E-16,0.898903149093028));
#2535=CARTESIAN_POINT('Origin',(-27.1538162925674,0.,0.));
#2536=CARTESIAN_POINT('',(-27.6022863156265,-2.20886334127906E-16,1.80367379624636));
#2537=CARTESIAN_POINT('',(-27.1538162925674,1.65485110277965E-16,1.35128847266969));
#2538=CARTESIAN_POINT('Origin',(-27.6022863156265,0.,0.));
#2539=CARTESIAN_POINT('Origin',(-28.1016442624067,0.,0.));
#2540=CARTESIAN_POINT('',(-28.6010022091869,-2.20886334127906E-16,1.80367379624636));
#2541=CARTESIAN_POINT('Origin',(-28.6010022091869,0.,0.));
#2542=CARTESIAN_POINT('',(-28.1016442624067,-2.20886334127906E-16,1.80367379624636));
#2543=CARTESIAN_POINT('Origin',(-28.6010022091869,0.,-1.9840612380693));
#2544=CARTESIAN_POINT('',(-28.6010022091869,-2.4297742445139E-16,1.9840612380693));
#2545=CARTESIAN_POINT('Origin',(-28.6010022091869,0.,0.));
#2546=CARTESIAN_POINT('Origin',(-22.120782962919,0.,0.));
#2547=CARTESIAN_POINT('',(-15.6405637166511,-2.4297742445139E-16,1.9840612380693));
#2548=CARTESIAN_POINT('Origin',(-15.6405637166511,0.,0.));
#2549=CARTESIAN_POINT('',(-22.120782962919,-2.4297742445139E-16,1.9840612380693));
#2550=CARTESIAN_POINT('',(-22.120782962919,-2.4297742445139E-16,1.9840612380693));
#2551=CARTESIAN_POINT('Origin',(-15.6405637166511,0.,-1.49577760563294));
#2552=CARTESIAN_POINT('',(-15.6405637166511,-1.83179925697468E-16,1.49577760563294));
#2553=CARTESIAN_POINT('Origin',(-15.6405637166511,0.,0.));
#2554=CARTESIAN_POINT('Origin',(-19.5773288456352,0.,0.));
#2555=CARTESIAN_POINT('',(-23.5140939746193,-1.83179925697468E-16,1.49577760563294));
#2556=CARTESIAN_POINT('Origin',(-23.5140939746193,0.,0.));
#2557=CARTESIAN_POINT('',(-19.5773288456352,-1.83179925697467E-16,1.49577760563294));
#2558=CARTESIAN_POINT('Origin',(-23.5140939746193,0.,-1.24385197034191));
#2559=CARTESIAN_POINT('',(-23.5140939746193,-1.52327933409234E-16,1.24385197034191));
#2560=CARTESIAN_POINT('Origin',(-23.5140939746193,0.,0.));
#2561=CARTESIAN_POINT('Origin',(-23.8926057114429,0.,0.));
#2562=CARTESIAN_POINT('',(-24.2711174482666,-1.52327933409234E-16,1.24385197034191));
#2563=CARTESIAN_POINT('Origin',(-24.2711174482666,0.,0.));
#2564=CARTESIAN_POINT('',(-23.8926057114429,-1.52327933409235E-16,1.24385197034191));
#2565=CARTESIAN_POINT('Origin',(-24.2711174482666,0.,0.));
#2566=CARTESIAN_POINT('',(0.,0.,0.));
#2567=CARTESIAN_POINT('Origin',(3.07820337465776,0.,0.));
#2568=CARTESIAN_POINT('',(6.37921955683583,-9.0534992499435E-16,7.3927431617401));
#2569=CARTESIAN_POINT('Origin',(6.37921955683583,0.,0.));
#2570=CARTESIAN_POINT('',(-0.222812807520296,-9.0534992499435E-16,7.3927431617401));
#2571=CARTESIAN_POINT('',(3.07820337465776,-9.0534992499435E-16,7.3927431617401));
#2572=CARTESIAN_POINT('Origin',(-0.222812807520296,0.,0.));
#2573=CARTESIAN_POINT('Origin',(6.62921955683583,0.,0.));
#2574=CARTESIAN_POINT('',(6.87921955683583,-8.44117585036982E-16,6.8927431617401));
#2575=CARTESIAN_POINT('',(6.62921955683583,8.74733755015666E-16,7.1427431617401));
#2576=CARTESIAN_POINT('Origin',(6.87921955683583,0.,0.));
#2577=CARTESIAN_POINT('Origin',(6.87921955683583,0.,-3.57153586442857));
#2578=CARTESIAN_POINT('',(6.87921955683583,-4.37386996441242E-16,3.57153586442857));
#2579=CARTESIAN_POINT('Origin',(6.87921955683583,0.,0.));
#2580=CARTESIAN_POINT('Origin',(6.36130355913187,0.,0.));
#2581=CARTESIAN_POINT('',(5.84338756142791,-3.11328111874601E-16,2.54218695620125));
#2582=CARTESIAN_POINT('Origin',(5.84338756142791,0.,0.));
#2583=CARTESIAN_POINT('',(6.36130355913187,-3.74357554157922E-16,3.05686141031491));
#2584=CARTESIAN_POINT('Origin',(5.84338756142791,0.,-1.93367516017024));
#2585=CARTESIAN_POINT('',(5.84338756142791,-2.36806909549322E-16,1.93367516017024));
#2586=CARTESIAN_POINT('Origin',(5.84338756142791,0.,0.));
#2587=CARTESIAN_POINT('Origin',(2.92894190571765,0.,0.));
#2588=CARTESIAN_POINT('',(0.0144962500073953,-2.36806909549322E-16,1.93367516017024));
#2589=CARTESIAN_POINT('Origin',(0.0144962500073953,0.,0.));
#2590=CARTESIAN_POINT('',(2.92894190571765,-2.36806909549323E-16,1.93367516017024));
#2591=CARTESIAN_POINT('Origin',(0.0144962500073953,0.,-3.68653879426857));
#2592=CARTESIAN_POINT('',(0.0144962500073954,-4.51470793433354E-16,3.68653879426857));
#2593=CARTESIAN_POINT('Origin',(0.0144962500073953,0.,0.));
#2594=CARTESIAN_POINT('Origin',(-0.501553695540098,0.,0.));
#2595=CARTESIAN_POINT('',(-1.01760364108759,-4.51470793433354E-16,3.68653879426857));
#2596=CARTESIAN_POINT('Origin',(-1.01760364108759,0.,0.));
#2597=CARTESIAN_POINT('',(-0.501553695540098,-4.51470793433355E-16,3.68653879426857));
#2598=CARTESIAN_POINT('Origin',(-1.01760364108759,0.,-3.10163618786504));
#2599=CARTESIAN_POINT('',(-1.01760364108759,-3.79840882958852E-16,3.10163618786504));
#2600=CARTESIAN_POINT('Origin',(-1.01760364108759,0.,0.));
#2601=CARTESIAN_POINT('Origin',(-1.65058882961282,0.,0.));
#2602=CARTESIAN_POINT('',(-2.28357401813804,-3.79840882958852E-16,3.10163618786504));
#2603=CARTESIAN_POINT('Origin',(-2.28357401813804,0.,0.));
#2604=CARTESIAN_POINT('',(-1.65058882961282,-3.79840882958852E-16,3.10163618786504));
#2605=CARTESIAN_POINT('Origin',(-2.41722174948925,0.,0.));
#2606=CARTESIAN_POINT('',(-2.55086948084045,-4.12944165277589E-16,3.37194500132688));
#2607=CARTESIAN_POINT('',(-2.41722174948925,3.9639252411822E-16,3.23679059459596));
#2608=CARTESIAN_POINT('Origin',(-2.55086948084045,0.,0.));
#2609=CARTESIAN_POINT('Origin',(-3.43730273109138,0.,0.));
#2610=CARTESIAN_POINT('',(-4.32373598134232,-4.12944165277589E-16,3.37194500132688));
#2611=CARTESIAN_POINT('Origin',(-4.32373598134232,0.,0.));
#2612=CARTESIAN_POINT('',(-3.43730273109138,-4.12944165277588E-16,3.37194500132688));
#2613=CARTESIAN_POINT('Origin',(-4.45085090816676,0.,0.));
#2614=CARTESIAN_POINT('',(-4.57796583499121,-4.44429333540845E-16,3.62904091081832));
#2615=CARTESIAN_POINT('',(-4.45085090816676,4.28686749409217E-16,3.5004929560726));
#2616=CARTESIAN_POINT('Origin',(-4.57796583499121,0.,0.));
#2617=CARTESIAN_POINT('Origin',(-4.57796583499121,0.,-5.34620669590443));
#2618=CARTESIAN_POINT('',(-4.57796583499121,-6.54721491771951E-16,5.34620669590443));
#2619=CARTESIAN_POINT('Origin',(-4.57796583499121,0.,0.));
#2620=CARTESIAN_POINT('Origin',(-4.32373598134232,0.,0.));
#2621=CARTESIAN_POINT('',(-4.06950612769342,-7.16295691404872E-16,5.84899819199777));
#2622=CARTESIAN_POINT('Origin',(-4.06950612769342,0.,0.));
#2623=CARTESIAN_POINT('',(-4.32373598134232,-6.85508591588412E-16,5.5976024439511));
#2624=CARTESIAN_POINT('Origin',(-2.6730798432382,0.,0.));
#2625=CARTESIAN_POINT('',(-1.27665355878298,-7.16295691404872E-16,5.84899819199777));
#2626=CARTESIAN_POINT('Origin',(-1.27665355878298,0.,0.));
#2627=CARTESIAN_POINT('',(-2.6730798432382,-7.16295691404872E-16,5.84899819199777));
#2628=CARTESIAN_POINT('Origin',(-1.27665355878298,0.,-6.35065042485944));
#2629=CARTESIAN_POINT('',(-1.27665355878298,-7.77730371530789E-16,6.35065042485944));
#2630=CARTESIAN_POINT('Origin',(-1.27665355878298,0.,0.));
#2631=CARTESIAN_POINT('Origin',(-0.749733183151639,0.,0.));
#2632=CARTESIAN_POINT('',(-0.749733183151639,-8.41540148262569E-16,6.87169679329977));
#2633=CARTESIAN_POINT('',(0.,0.,0.));
#2634=CARTESIAN_POINT('Origin',(-9.8399217662475,0.,0.));
#2635=CARTESIAN_POINT('',(-9.94097953629964,-1.83179925697468E-16,1.49577760563294));
#2636=CARTESIAN_POINT('Origin',(-9.94097953629964,0.,0.));
#2637=CARTESIAN_POINT('',(-9.73886399619536,-1.41182176522558E-16,1.15283995859749));
#2638=CARTESIAN_POINT('',(-9.8399217662475,1.62181051110013E-16,1.32430878211522));
#2639=CARTESIAN_POINT('Origin',(-9.73886399619536,0.,0.));
#2640=CARTESIAN_POINT('Origin',(-9.36350656457311,0.,0.));
#2641=CARTESIAN_POINT('',(-8.98814913295086,-1.41182176522558E-16,1.15283995859749));
#2642=CARTESIAN_POINT('Origin',(-8.98814913295086,0.,0.));
#2643=CARTESIAN_POINT('',(-9.36350656457311,-1.41182176522558E-16,1.15283995859749));
#2644=CARTESIAN_POINT('Origin',(-8.98814913295086,0.,-1.99455837231036));
#2645=CARTESIAN_POINT('',(-8.98814913295086,-2.44262952636244E-16,1.99455837231036));
#2646=CARTESIAN_POINT('Origin',(-8.98814913295086,0.,0.));
#2647=CARTESIAN_POINT('Origin',(-8.90180302208485,0.,0.));
#2648=CARTESIAN_POINT('',(-8.81545691121883,-2.83677232469619E-16,2.3164003912567));
#2649=CARTESIAN_POINT('Origin',(-8.81545691121883,0.,0.));
#2650=CARTESIAN_POINT('',(-8.90180302208485,-2.63970092552932E-16,2.15547938178353));
#2651=CARTESIAN_POINT('Origin',(-5.99766844795496,0.,0.));
#2652=CARTESIAN_POINT('',(-3.17987998469109,-2.83677232469619E-16,2.3164003912567));
#2653=CARTESIAN_POINT('Origin',(-3.17987998469109,0.,0.));
#2654=CARTESIAN_POINT('',(-5.99766844795496,-2.83677232469619E-16,2.3164003912567));
#2655=CARTESIAN_POINT('Origin',(-3.09467275323448,0.,0.));
#2656=CARTESIAN_POINT('',(-3.00946552177786,-2.47996687610391E-16,2.02504663208246));
#2657=CARTESIAN_POINT('',(-3.09467275323448,2.65836960040005E-16,2.17072351166958));
#2658=CARTESIAN_POINT('Origin',(-3.00946552177786,0.,0.));
#2659=CARTESIAN_POINT('Origin',(-3.00946552177786,0.,-0.94209020647254));
#2660=CARTESIAN_POINT('',(-3.00946552177786,-1.15372775586467E-16,0.94209020647254));
#2661=CARTESIAN_POINT('Origin',(-3.00946552177786,0.,0.));
#2662=CARTESIAN_POINT('Origin',(-3.89726990114842,0.,0.));
#2663=CARTESIAN_POINT('',(-4.78507428051899,-1.15372775586467E-16,0.94209020647254));
#2664=CARTESIAN_POINT('Origin',(-4.78507428051899,0.,0.));
#2665=CARTESIAN_POINT('',(-3.89726990114842,-1.15372775586467E-16,0.94209020647254));
#2666=CARTESIAN_POINT('Origin',(-4.78507428051899,0.,0.));
#2667=CARTESIAN_POINT('Origin',(-16.9835276458929,0.,-1.02706997925809));
#2668=CARTESIAN_POINT('',(-16.9835276458929,-1.25779796259876E-16,1.02706997925809));
#2669=CARTESIAN_POINT('Origin',(-16.9835276458929,0.,0.));
#2670=CARTESIAN_POINT('Origin',(-16.7880966836618,0.,0.));
#2671=CARTESIAN_POINT('',(-16.5926657214308,-1.25779796259876E-16,1.02706997925809));
#2672=CARTESIAN_POINT('Origin',(-16.5926657214308,0.,0.));
#2673=CARTESIAN_POINT('',(-16.7880966836618,-1.25779796259876E-16,1.02706997925809));
#2674=CARTESIAN_POINT('Origin',(-16.5926657214308,0.,-1.49577760563294));
#2675=CARTESIAN_POINT('',(-16.5926657214308,-1.83179925697468E-16,1.49577760563294));
#2676=CARTESIAN_POINT('Origin',(-16.5926657214308,0.,0.));
#2677=CARTESIAN_POINT('Origin',(-13.2668226288652,0.,0.));
#2678=CARTESIAN_POINT('',(-13.2668226288652,-1.83179925697467E-16,1.49577760563294));
#2679=CARTESIAN_POINT('',(0.,0.,0.));
#2680=CARTESIAN_POINT('Origin',(-2.40309980332239,0.,0.));
#2681=CARTESIAN_POINT('',(-2.28588076473159,-2.83677232469619E-16,2.3164003912567));
#2682=CARTESIAN_POINT('Origin',(-2.28588076473159,0.,0.));
#2683=CARTESIAN_POINT('',(-2.52031884191318,-2.52715675294263E-16,2.06358009076751));
#2684=CARTESIAN_POINT('',(-2.40309980332239,-2.68196453881941E-16,2.1899902410121));
#2685=CARTESIAN_POINT('Origin',(-2.52031884191318,0.,0.));
#2686=CARTESIAN_POINT('Origin',(-1.71486702953379,0.,0.));
#2687=CARTESIAN_POINT('',(-1.14385329433599,-2.83677232469619E-16,2.3164003912567));
#2688=CARTESIAN_POINT('Origin',(-1.14385329433599,0.,0.));
#2689=CARTESIAN_POINT('',(-1.71486702953379,-2.83677232469619E-16,2.3164003912567));
#2690=CARTESIAN_POINT('Origin',(-1.14385329433599,0.,-1.99619194538056));
#2691=CARTESIAN_POINT('',(-1.14385329433599,-2.44463007639404E-16,1.99619194538056));
#2692=CARTESIAN_POINT('Origin',(-1.14385329433599,0.,0.));
#2693=CARTESIAN_POINT('Origin',(-0.89153499844287,0.,0.));
#2694=CARTESIAN_POINT('',(-0.639216702549746,-2.44463007639404E-16,1.99619194538056));
#2695=CARTESIAN_POINT('Origin',(-0.639216702549746,0.,0.));
#2696=CARTESIAN_POINT('',(-0.89153499844287,-2.44463007639403E-16,1.99619194538056));
#2697=CARTESIAN_POINT('Origin',(-0.639216702549746,0.,-2.3164003912567));
#2698=CARTESIAN_POINT('',(-0.639216702549746,-2.83677232469619E-16,2.3164003912567));
#2699=CARTESIAN_POINT('Origin',(-0.639216702549746,0.,0.));
#2700=CARTESIAN_POINT('Origin',(-0.312360226271176,0.,0.));
#2701=CARTESIAN_POINT('',(0.0144962500073953,-2.83677232469619E-16,2.3164003912567));
#2702=CARTESIAN_POINT('Origin',(0.0144962500073953,0.,0.));
#2703=CARTESIAN_POINT('',(-0.312360226271176,-2.83677232469619E-16,2.3164003912567));
#2704=CARTESIAN_POINT('Origin',(0.0144962500073953,0.,-1.93367516017024));
#2705=CARTESIAN_POINT('',(0.0144962500073953,-2.36806909549322E-16,1.93367516017024));
#2706=CARTESIAN_POINT('Origin',(0.0144962500073953,0.,0.));
#2707=CARTESIAN_POINT('Origin',(0.00924228164886909,0.,0.));
#2708=CARTESIAN_POINT('',(0.00398831329034288,-1.42161846754312E-16,1.16083957311848));
#2709=CARTESIAN_POINT('Origin',(0.00398831329034288,0.,0.));
#2710=CARTESIAN_POINT('',(0.00924228164886909,-1.89484378151818E-16,1.54725736664436));
#2711=CARTESIAN_POINT('Origin',(-1.25816526431142,0.,0.));
#2712=CARTESIAN_POINT('',(-2.52031884191318,-1.42161846754312E-16,1.16083957311848));
#2713=CARTESIAN_POINT('Origin',(-2.52031884191318,0.,0.));
#2714=CARTESIAN_POINT('',(-1.25816526431142,-1.42161846754313E-16,1.16083957311848));
#2715=CARTESIAN_POINT('Origin',(-2.52031884191318,0.,-2.06358009076751));
#2716=CARTESIAN_POINT('',(0.,0.,0.));
#2717=CARTESIAN_POINT('Ctrl Pts',(-12.4302293937643,-1.29488419085615,6.08893179912409));
#2718=CARTESIAN_POINT('Ctrl Pts',(-12.5942554551731,-1.29488414718856,6.08893179050175));
#2719=CARTESIAN_POINT('Ctrl Pts',(-12.9434041993798,-1.2294328459869,6.10376298255976));
#2720=CARTESIAN_POINT('Ctrl Pts',(-13.2352719744654,-1.0316590890245,6.14035711678102));
#2721=CARTESIAN_POINT('Ctrl Pts',(-13.4652582677038,-0.804188184632238,
6.1743411575965));
#2722=CARTESIAN_POINT('Ctrl Pts',(-13.6645706157926,-0.50626213886193,6.21083535170997));
#2723=CARTESIAN_POINT('Ctrl Pts',(-13.7634101258885,-4.55193504007075E-5,
6.23259369899848));
#2724=CARTESIAN_POINT('Ctrl Pts',(-13.6645494097846,0.506350803091124,6.21079370032761));
#2725=CARTESIAN_POINT('Ctrl Pts',(-13.4651211785068,0.804025993881401,6.17427297012694));
#2726=CARTESIAN_POINT('Ctrl Pts',(-13.2354048303999,1.03253237976219,6.14014393621034));
#2727=CARTESIAN_POINT('Ctrl Pts',(-13.0895391630103,1.13181896559648,6.12197280773622));
#2728=CARTESIAN_POINT('Ctrl Pts',(-12.7690246025484,1.26358725386243,6.09603285881286));
#2729=CARTESIAN_POINT('Ctrl Pts',(-12.5943534667659,1.29612320858372,6.08887111511598));
#2730=CARTESIAN_POINT('Ctrl Pts',(-12.2661214257273,1.29612709871105,6.08886919819022));
#2731=CARTESIAN_POINT('Ctrl Pts',(-12.0914504696733,1.26359486961962,6.09602904830329));
#2732=CARTESIAN_POINT('Ctrl Pts',(-11.7709375208824,1.13183595785232,6.12196443982891));
#2733=CARTESIAN_POINT('Ctrl Pts',(-11.6250715919502,1.03254971804437,6.14013512447093));
#2734=CARTESIAN_POINT('Ctrl Pts',(-11.395360898952,0.804063499952342,6.17425479916453));
#2735=CARTESIAN_POINT('Ctrl Pts',(-11.1959336454396,0.506396277936275,6.2107637521937));
#2736=CARTESIAN_POINT('Ctrl Pts',(-11.0970937797084,6.1156379640301E-5,
6.23254880516501));
#2737=CARTESIAN_POINT('Ctrl Pts',(-11.1959237146699,-0.506186673149979,
6.21076962890895));
#2738=CARTESIAN_POINT('Ctrl Pts',(-11.3952900549715,-0.803952284531892,
6.17425879944784));
#2739=CARTESIAN_POINT('Ctrl Pts',(-11.6251494839037,-1.03184033349927,6.14017845211199));
#2740=CARTESIAN_POINT('Ctrl Pts',(-11.7709627360902,-1.13109996217884,6.12198310555546));
#2741=CARTESIAN_POINT('Ctrl Pts',(-12.0914571818659,-1.26265113550208,6.09609663062554));
#2742=CARTESIAN_POINT('Ctrl Pts',(-12.2662033433641,-1.29488420847439,6.08893179144279));
#2743=CARTESIAN_POINT('Ctrl Pts',(-12.4302293937643,-1.29488419085615,6.08893179912409));
#2744=CARTESIAN_POINT('Ctrl Pts',(-12.4302293937643,-1.19653776428921,6.00731901992712));
#2745=CARTESIAN_POINT('Ctrl Pts',(-12.5835320638101,-1.19669374251964,6.00734981845634));
#2746=CARTESIAN_POINT('Ctrl Pts',(-12.9098993488334,-1.13385554423326,6.02032135745683));
#2747=CARTESIAN_POINT('Ctrl Pts',(-13.1794444923897,-0.948175876780826,
6.05212160800709));
#2748=CARTESIAN_POINT('Ctrl Pts',(-13.3904188730421,-0.736106912634719,
6.08151671837308));
#2749=CARTESIAN_POINT('Ctrl Pts',(-13.571358399148,-0.461107396153454,6.11288518823509));
#2750=CARTESIAN_POINT('Ctrl Pts',(-13.6598647804087,-4.77349200694727E-5,
6.13145209579345));
#2751=CARTESIAN_POINT('Ctrl Pts',(-13.5713351984267,0.461201603549934,6.11284433707963));
#2752=CARTESIAN_POINT('Ctrl Pts',(-13.3902865479058,0.73593723140633,6.0814466719145));
#2753=CARTESIAN_POINT('Ctrl Pts',(-13.1795657386676,0.949053789500503,6.05191117775911));
#2754=CARTESIAN_POINT('Ctrl Pts',(-13.0448959816465,1.04218619158655,6.03613258011903));
#2755=CARTESIAN_POINT('Ctrl Pts',(-12.7468860466288,1.16681531246955,6.01352866653896));
#2756=CARTESIAN_POINT('Ctrl Pts',(-12.5836668315555,1.19776542529252,6.00726540810815));
#2757=CARTESIAN_POINT('Ctrl Pts',(-12.2768080336065,1.19776973044414,6.00726351057582));
#2758=CARTESIAN_POINT('Ctrl Pts',(-12.1135891439065,1.16682230335479,6.01352482644386));
#2759=CARTESIAN_POINT('Ctrl Pts',(-11.8155804810902,1.04220414880451,6.03612425707734));
#2760=CARTESIAN_POINT('Ctrl Pts',(-11.6809112042485,0.949069004361932,6.05190226572165));
#2761=CARTESIAN_POINT('Ctrl Pts',(-11.4701945190351,0.735978790867167,6.08142869039248));
#2762=CARTESIAN_POINT('Ctrl Pts',(-11.2891496988235,0.461239711890714,6.11281404103072));
#2763=CARTESIAN_POINT('Ctrl Pts',(-11.2006363964354,6.98177936070269E-5,
6.13140771052673));
#2764=CARTESIAN_POINT('Ctrl Pts',(-11.2891410326498,-0.461052166154195,
6.11281851072142));
#2765=CARTESIAN_POINT('Ctrl Pts',(-11.4701207397339,-0.735837035061057,
6.08143595189992));
#2766=CARTESIAN_POINT('Ctrl Pts',(-11.6809938866623,-0.948407049105129,
6.05194059445036));
#2767=CARTESIAN_POINT('Ctrl Pts',(-11.8156020963373,-1.04142835561581,6.03614993606957));
#2768=CARTESIAN_POINT('Ctrl Pts',(-12.1135988587321,-1.16591750294593,6.01358226833267));
#2769=CARTESIAN_POINT('Ctrl Pts',(-12.2768874021684,-1.1964748328885,6.00734645713312));
#2770=CARTESIAN_POINT('Ctrl Pts',(-12.4302293937643,-1.19653776428921,6.00731901992712));
#2771=CARTESIAN_POINT('Ctrl Pts',(-12.4302293937643,-1.09819133772228,5.92570624073015));
#2772=CARTESIAN_POINT('Ctrl Pts',(-12.5728763428205,-1.09803515711868,5.92567540224153));
#2773=CARTESIAN_POINT('Ctrl Pts',(-12.876321077954,-1.0387969727173,5.93681987239533));
#2774=CARTESIAN_POINT('Ctrl Pts',(-13.1236914762163,-0.863950043440302,
5.96385707568949));
#2775=CARTESIAN_POINT('Ctrl Pts',(-13.3155790887801,-0.668255697608592,
5.98863521528464));
#2776=CARTESIAN_POINT('Ctrl Pts',(-13.4781865651095,-0.415776757496831,
6.0149151254311));
#2777=CARTESIAN_POINT('Ctrl Pts',(-13.5561689964186,4.21654537423543E-5,
6.03022023183205));
#2778=CARTESIAN_POINT('Ctrl Pts',(-13.478150753931,0.415977680530914,6.01488398902043));
#2779=CARTESIAN_POINT('Ctrl Pts',(-13.315393862027,0.668313266257187,5.98858257490239));
#2780=CARTESIAN_POINT('Ctrl Pts',(-13.1237891612582,0.864807186170974,5.96371046903562));
#2781=CARTESIAN_POINT('Ctrl Pts',(-13.000238685325,0.952440693384399,5.95029853437126));
#2782=CARTESIAN_POINT('Ctrl Pts',(-12.7247805462859,1.06962276776914,5.93103239143954));
#2783=CARTESIAN_POINT('Ctrl Pts',(-12.5729657038671,1.09913712296315,5.92566846199632));
#2784=CARTESIAN_POINT('Ctrl Pts',(-12.2875198521031,1.09913697678003,5.92566694755825));
#2785=CARTESIAN_POINT('Ctrl Pts',(-12.1357051736444,1.06962385288842,5.93102945126453));
#2786=CARTESIAN_POINT('Ctrl Pts',(-11.8602500197414,0.952440909619879,5.95029196307193));
#2787=CARTESIAN_POINT('Ctrl Pts',(-11.7366984580338,0.864810198814481,5.96370370664712));
#2788=CARTESIAN_POINT('Ctrl Pts',(-11.5451044624593,0.668312166922651,5.98856820249765));
#2789=CARTESIAN_POINT('Ctrl Pts',(-11.3823489586879,0.415979415085571,6.01486124976089));
#2790=CARTESIAN_POINT('Ctrl Pts',(-11.3043647489821,4.76005030248672E-5,
6.0301844356551));
#2791=CARTESIAN_POINT('Ctrl Pts',(-11.3823356020908,-0.415784531254904,
6.0148658425333));
#2792=CARTESIAN_POINT('Ctrl Pts',(-11.5450254725926,-0.66823389832439,5.98856817993586));
#2793=CARTESIAN_POINT('Ctrl Pts',(-11.7367782945029,-0.864224843995978,
5.96372965668036));
#2794=CARTESIAN_POINT('Ctrl Pts',(-11.8602868211275,-0.951940725192759,
5.9502902505237));
#2795=CARTESIAN_POINT('Ctrl Pts',(-12.1357015099293,-1.06885043095419,5.9310779680282));
#2796=CARTESIAN_POINT('Ctrl Pts',(-12.2876218172759,-1.09825435077303,5.92567876792588));
#2797=CARTESIAN_POINT('Ctrl Pts',(-12.4302293937643,-1.09819133772228,5.92570624073015));
#2798=CARTESIAN_POINT('Ctrl Pts',(-12.4302293937643,-0.999844911155348,
5.84409346153317));
#2799=CARTESIAN_POINT('Ctrl Pts',(-12.5621528929196,-0.999845157446748,
5.8440935101644));
#2800=CARTESIAN_POINT('Ctrl Pts',(-12.8428162909195,-0.943219222239121,
5.85337829907391));
#2801=CARTESIAN_POINT('Ctrl Pts',(-13.0678639297245,-0.780467473596644,
5.87562159202221));
#2802=CARTESIAN_POINT('Ctrl Pts',(-13.2407396944553,-0.600174226601641,
5.89581082542398));
#2803=CARTESIAN_POINT('Ctrl Pts',(-13.3849743135323,-0.370622166946112,
5.91696497917002));
#2804=CARTESIAN_POINT('Ctrl Pts',(-13.4526237810749,3.98701997180173E-5,
5.92907870670656));
#2805=CARTESIAN_POINT('Ctrl Pts',(-13.3849365168234,0.370828545628829,5.9169346352748));
#2806=CARTESIAN_POINT('Ctrl Pts',(-13.2405592816462,0.60022410171192,5.89575630938757));
#2807=CARTESIAN_POINT('Ctrl Pts',(-13.0679500154482,0.781329260274485,5.87547768285996));
#2808=CARTESIAN_POINT('Ctrl Pts',(-12.9555955161712,0.862808016885863,5.86445830140649));
#2809=CARTESIAN_POINT('Ctrl Pts',(-12.7026419617718,0.972851190216686,5.84852819231695));
#2810=CARTESIAN_POINT('Ctrl Pts',(-12.5622790811935,1.00077957368287,5.84406274740993));
#2811=CARTESIAN_POINT('Ctrl Pts',(-12.2982064381739,1.00077984673363,5.84406125205068));
#2812=CARTESIAN_POINT('Ctrl Pts',(-12.157843867466,0.972851655032226,5.84852522175233));
#2813=CARTESIAN_POINT('Ctrl Pts',(-11.9048929569576,0.862809214264935,5.86445177349625));
#2814=CARTESIAN_POINT('Ctrl Pts',(-11.7925381156245,0.781330158215836,5.87547081822711));
#2815=CARTESIAN_POINT('Ctrl Pts',(-11.6199380165194,0.600227096175383,5.89574212346506));
#2816=CARTESIAN_POINT('Ctrl Pts',(-11.4755650265989,0.370822938771694,5.91691154126233));
#2817=CARTESIAN_POINT('Ctrl Pts',(-11.4079072050394,5.62886284334987E-5,
5.92904341210635));
#2818=CARTESIAN_POINT('Ctrl Pts',(-11.4755529397492,-0.370650139420631,
5.91691472568658));
#2819=CARTESIAN_POINT('Ctrl Pts',(-11.6198560933002,-0.600118205853443,
5.89574537124953));
#2820=CARTESIAN_POINT('Ctrl Pts',(-11.7926227491599,-0.780792207451304,
5.87549177573183));
#2821=CARTESIAN_POINT('Ctrl Pts',(-11.9049261421322,-0.862268959482245,
5.86445710397538));
#2822=CARTESIAN_POINT('Ctrl Pts',(-12.1578432205544,-0.972117086837851,
5.84856359703126));
#2823=CARTESIAN_POINT('Ctrl Pts',(-12.2983058325198,-0.99984481178595,5.84409350485683));
#2824=CARTESIAN_POINT('Ctrl Pts',(-12.4302293937643,-0.999844911155348,
5.84409346153317));
#2825=CARTESIAN_POINT('',(-12.4302293937643,-1.29485665783831,6.08890895085005));
#2826=CARTESIAN_POINT('',(-12.4302293937643,-1.,5.84422216200635));
#2827=CARTESIAN_POINT('',(-12.4302293937643,-1.29485665783831,6.08890895085005));
#2828=CARTESIAN_POINT('',(-13.4302255152826,6.09774944770533E-5,5.92519355911023));
#2829=CARTESIAN_POINT('Ctrl Pts',(-12.4302293937643,-0.999999999999999,
5.84422216200635));
#2830=CARTESIAN_POINT('Ctrl Pts',(-12.4592558850193,-0.999999999999999,
5.84422216200635));
#2831=CARTESIAN_POINT('Ctrl Pts',(-12.488694554397,-0.998732061148834,5.84444691869061));
#2832=CARTESIAN_POINT('Ctrl Pts',(-12.5183095428325,-0.996113390804545,
5.84488149270083));
#2833=CARTESIAN_POINT('Ctrl Pts',(-12.5476999043046,-0.993514582833954,
5.84531277050715));
#2834=CARTESIAN_POINT('Ctrl Pts',(-12.5772632652184,-0.989585307459082,
5.84595069482016));
#2835=CARTESIAN_POINT('Ctrl Pts',(-12.6067599503988,-0.984295160292032,
5.84678066365066));
#2836=CARTESIAN_POINT('Ctrl Pts',(-12.6361724957008,-0.979020103374498,
5.84760826497863));
#2837=CARTESIAN_POINT('Ctrl Pts',(-12.6655180670433,-0.972391909338808,
5.84862681676514));
#2838=CARTESIAN_POINT('Ctrl Pts',(-12.6945598901648,-0.964432158667805,
5.84982184162226));
#2839=CARTESIAN_POINT('Ctrl Pts',(-12.7235845842301,-0.956477102709557,
5.85101616164594));
#2840=CARTESIAN_POINT('Ctrl Pts',(-12.7523052168835,-0.947192192568073,
5.85238674663169));
#2841=CARTESIAN_POINT('Ctrl Pts',(-12.7804964410769,-0.936649878859193,
5.85391914479304));
#2842=CARTESIAN_POINT('Ctrl Pts',(-12.7968729154253,-0.930525776945672,
5.85480932533323));
#2843=CARTESIAN_POINT('Ctrl Pts',(-12.8130709993127,-0.923978305979963,
5.85575411017152));
#2844=CARTESIAN_POINT('Ctrl Pts',(-12.8290495544449,-0.917029159533509,
5.85675066634454));
#2845=CARTESIAN_POINT('Ctrl Pts',(-12.8572091311095,-0.90478243130972,5.85850693277305));
#2846=CARTESIAN_POINT('Ctrl Pts',(-12.8847319564144,-0.89126554770641,5.86042399200011));
#2847=CARTESIAN_POINT('Ctrl Pts',(-12.9114199263146,-0.876616034181418,
5.86245467738282));
#2848=CARTESIAN_POINT('Ctrl Pts',(-12.9382815849427,-0.861871179745247,
5.86449857872621));
#2849=CARTESIAN_POINT('Ctrl Pts',(-12.9642969455781,-0.845979342985271,
5.86665759002513));
#2850=CARTESIAN_POINT('Ctrl Pts',(-12.9892973901898,-0.829121809731686,
5.86888361773069));
#2851=CARTESIAN_POINT('Ctrl Pts',(-13.0144268115212,-0.812177308851183,
5.87112112946207));
#2852=CARTESIAN_POINT('Ctrl Pts',(-13.0385304149824,-0.794257687420666,
5.87342635085594));
#2853=CARTESIAN_POINT('Ctrl Pts',(-13.0614777313691,-0.775580773531183,
5.87575044017624));
#2854=CARTESIAN_POINT('Ctrl Pts',(-13.0847063998404,-0.7566748660387,5.87810302465319));
#2855=CARTESIAN_POINT('Ctrl Pts',(-13.1067499553324,-0.73699361188813,5.88047494256405));
#2856=CARTESIAN_POINT('Ctrl Pts',(-13.12752017916,-0.716788365281066,5.88281553354217));
#2857=CARTESIAN_POINT('Ctrl Pts',(-13.1365883945672,-0.707966817178806,
5.88383742831548));
#2858=CARTESIAN_POINT('Ctrl Pts',(-13.1454145186503,-0.699045653989259,
5.88485335164735));
#2859=CARTESIAN_POINT('Ctrl Pts',(-13.1539941405822,-0.690046803676091,
5.88585908744382));
#2860=CARTESIAN_POINT('Ctrl Pts',(-13.1726519250301,-0.670477338872932,
5.88804622364294));
#2861=CARTESIAN_POINT('Ctrl Pts',(-13.1907859755752,-0.64986192549443,5.89025601762883));
#2862=CARTESIAN_POINT('Ctrl Pts',(-13.2081852637323,-0.628318919325442,
5.89245033006015));
#2863=CARTESIAN_POINT('Ctrl Pts',(-13.2254454107646,-0.606948191360311,
5.89462709469886));
#2864=CARTESIAN_POINT('Ctrl Pts',(-13.2419819765234,-0.584665033083303,
5.89678862440316));
#2865=CARTESIAN_POINT('Ctrl Pts',(-13.2576215487824,-0.561624627143889,
5.89889768752854));
#2866=CARTESIAN_POINT('Ctrl Pts',(-13.2732257818358,-0.538636283347225,
5.90100198501107));
#2867=CARTESIAN_POINT('Ctrl Pts',(-13.2879366304041,-0.514894595696598,
5.90305405275394));
#2868=CARTESIAN_POINT('Ctrl Pts',(-13.301621703492,-0.490586834869639,5.90501691092882));
#2869=CARTESIAN_POINT('Ctrl Pts',(-13.3153299106845,-0.466237982681504,
5.90698308724208));
#2870=CARTESIAN_POINT('Ctrl Pts',(-13.3280085421283,-0.441321716069898,
5.90885975212154));
#2871=CARTESIAN_POINT('Ctrl Pts',(-13.3395704076334,-0.416051583935773,
5.91060973788262));
#2872=CARTESIAN_POINT('Ctrl Pts',(-13.3470788440547,-0.399640808321703,
5.91174620299885));
#2873=CARTESIAN_POINT('Ctrl Pts',(-13.3541172575866,-0.38308129324033,5.91282924266107));
#2874=CARTESIAN_POINT('Ctrl Pts',(-13.3606728897663,-0.366435397781884,
5.9138486772792));
#2875=CARTESIAN_POINT('Ctrl Pts',(-13.3752589610175,-0.32939881449871,5.91611688659423));
#2876=CARTESIAN_POINT('Ctrl Pts',(-13.3874617255085,-0.291938214172012,
5.91807022026964));
#2877=CARTESIAN_POINT('Ctrl Pts',(-13.3973781083062,-0.254211258523014,
5.91968556259891));
#2878=CARTESIAN_POINT('Ctrl Pts',(-13.4075677866282,-0.215444547921944,
5.9213454237651));
#2879=CARTESIAN_POINT('Ctrl Pts',(-13.4153439945548,-0.17639549147079,5.9226484067786));
#2880=CARTESIAN_POINT('Ctrl Pts',(-13.4207734325054,-0.137195143188463,
5.92356943156943));
#2881=CARTESIAN_POINT('Ctrl Pts',(-13.4263319366763,-0.0970629414001139,
5.92451235055809));
#2882=CARTESIAN_POINT('Ctrl Pts',(-13.4294312404248,-0.0567708233405655,
5.92505493599733));
#2883=CARTESIAN_POINT('Ctrl Pts',(-13.4300942971141,-0.0164370024408991,
5.92517027638565));
#2884=CARTESIAN_POINT('Ctrl Pts',(-13.4301846903816,-0.0109383687327478,
5.92518600052318));
#2885=CARTESIAN_POINT('Ctrl Pts',(-13.430229727278,-0.00543894523112027,
5.92519378415999));
#2886=CARTESIAN_POINT('Ctrl Pts',(-13.4302293919052,6.09777308642567E-5,
5.92519355911023));
#2887=CARTESIAN_POINT('Ctrl Pts',(-13.4302255152826,6.09774944770533E-5,
5.92519355911023));
#2888=CARTESIAN_POINT('Ctrl Pts',(-13.4302192163544,0.123659830589739,5.92518850158483));
#2889=CARTESIAN_POINT('Ctrl Pts',(-13.3850835123617,0.370899744283506,5.91708909795873));
#2890=CARTESIAN_POINT('Ctrl Pts',(-13.2406772931872,0.600331475536471,5.89590269316437));
#2891=CARTESIAN_POINT('Ctrl Pts',(-13.0680380717591,0.781460902655162,5.87561682282398));
#2892=CARTESIAN_POINT('Ctrl Pts',(-12.9556659168855,0.862949364547602,5.86459366841997));
#2893=CARTESIAN_POINT('Ctrl Pts',(-12.702676873511,0.973003795928843,5.84865829852133));
#2894=CARTESIAN_POINT('Ctrl Pts',(-12.5622959336324,1.00093468029201,5.8441914367352));
#2895=CARTESIAN_POINT('Ctrl Pts',(-12.2981895857838,1.00093495268569,5.84418994134556));
#2896=CARTESIAN_POINT('Ctrl Pts',(-12.1578089555458,0.97300426172696,5.84865532800387));
#2897=CARTESIAN_POINT('Ctrl Pts',(-11.9048225565987,0.862950560394959,5.86458714043989));
#2898=CARTESIAN_POINT('Ctrl Pts',(-11.7924500584981,0.781461803939683,5.8756099583505));
#2899=CARTESIAN_POINT('Ctrl Pts',(-11.6198200065818,0.6003344635829,5.89588850694494));
#2900=CARTESIAN_POINT('Ctrl Pts',(-11.4754180281628,0.370894149027576,5.91706600449914));
#2901=CARTESIAN_POINT('Ctrl Pts',(-11.4077439220855,5.62749531760182E-5,
5.929202908));
#2902=CARTESIAN_POINT('Ctrl Pts',(-11.4754059393156,-0.370721314874449,
5.91706919114304));
#2903=CARTESIAN_POINT('Ctrl Pts',(-11.6197380879902,-0.600225621472355,
5.89589174958094));
#2904=CARTESIAN_POINT('Ctrl Pts',(-11.7925346844751,-0.780923778396437,
5.87563092373439));
#2905=CARTESIAN_POINT('Ctrl Pts',(-11.9048557474604,-0.862410368540219,
5.86459245984095));
#2906=CARTESIAN_POINT('Ctrl Pts',(-12.1578083038904,-0.972269632184938,
5.84869371927455));
#2907=CARTESIAN_POINT('Ctrl Pts',(-12.298288984163,-1.,5.84422216200635));
#2908=CARTESIAN_POINT('Ctrl Pts',(-12.4302293937643,-1.,5.84422216200635));
#2909=CARTESIAN_POINT('',(-11.1302593513097,-3.3449167263952E-15,6.22506754791384));
#2910=CARTESIAN_POINT('Ctrl Pts',(-12.4302293937643,-1.29485665783831,6.08890895085005));
#2911=CARTESIAN_POINT('Ctrl Pts',(-12.3550509351911,-1.29485665783831,6.08890895085005));
#2912=CARTESIAN_POINT('Ctrl Pts',(-12.2791894522468,-1.28803385899595,6.09037004805683));
#2913=CARTESIAN_POINT('Ctrl Pts',(-12.1289044531663,-1.26195566431335,6.09582777868059));
#2914=CARTESIAN_POINT('Ctrl Pts',(-12.0533392104996,-1.24213987866781,6.09994033109874));
#2915=CARTESIAN_POINT('Ctrl Pts',(-11.9315538541034,-1.19807725994036,6.10871557265866));
#2916=CARTESIAN_POINT('Ctrl Pts',(-11.8841287877011,-1.17740270840153,6.1127532723677));
#2917=CARTESIAN_POINT('Ctrl Pts',(-11.7773853504172,-1.12312910404621,6.12299260884751));
#2918=CARTESIAN_POINT('Ctrl Pts',(-11.7187497040409,-1.08726612645883,6.12951525526529));
#2919=CARTESIAN_POINT('Ctrl Pts',(-11.6017107249225,-1.00275397201799,6.14393994768209));
#2920=CARTESIAN_POINT('Ctrl Pts',(-11.5425195814749,-0.951920261192589,
6.15210896307454));
#2921=CARTESIAN_POINT('Ctrl Pts',(-11.430697412608,-0.835085988005597,6.16911299212126));
#2922=CARTESIAN_POINT('Ctrl Pts',(-11.3777994433336,-0.766398454187795,
6.17813694724593));
#2923=CARTESIAN_POINT('Ctrl Pts',(-11.270636406155,-0.596492970430275,6.19720348504624));
#2924=CARTESIAN_POINT('Ctrl Pts',(-11.1895796685093,-0.441508390314537,
6.21286406982716));
#2925=CARTESIAN_POINT('Ctrl Pts',(-11.1373062258032,-0.156727656024724,
6.22357399872114));
#2926=CARTESIAN_POINT('Ctrl Pts',(-11.1302626056501,-0.0783821040661418,
6.22506754791384));
#2927=CARTESIAN_POINT('Ctrl Pts',(-11.1302593513097,-3.34492582124604E-15,
6.22506754791384));
#2928=CARTESIAN_POINT('',(-13.730193598416,-1.52223171728111E-5,6.22506754789523));
#2929=CARTESIAN_POINT('Ctrl Pts',(-11.1302593513097,-3.34492582124604E-15,
6.22506754791384));
#2930=CARTESIAN_POINT('Ctrl Pts',(-11.1302591508642,0.00482780934498283,
6.22506754791384));
#2931=CARTESIAN_POINT('Ctrl Pts',(-11.1302855894096,0.00965575735666793,
6.22506193146085));
#2932=CARTESIAN_POINT('Ctrl Pts',(-11.1312380214286,0.0961986804474738,
6.22486057533084));
#2933=CARTESIAN_POINT('Ctrl Pts',(-11.1397779605581,0.177490219299905,6.22305207271077));
#2934=CARTESIAN_POINT('Ctrl Pts',(-11.1965749654798,0.457465808422005,6.2114605744672));
#2935=CARTESIAN_POINT('Ctrl Pts',(-11.2779391678912,0.614760694236416,6.19569689193407));
#2936=CARTESIAN_POINT('Ctrl Pts',(-11.4177773665018,0.822304084339778,6.17123945541837));
#2937=CARTESIAN_POINT('Ctrl Pts',(-11.4776318829417,0.885564567494429,6.16184436313107));
#2938=CARTESIAN_POINT('Ctrl Pts',(-11.6265144893125,1.03369488241838,6.13975499030251));
#2939=CARTESIAN_POINT('Ctrl Pts',(-11.769285484611,1.12926516148223,6.12213126261246));
#2940=CARTESIAN_POINT('Ctrl Pts',(-11.9958937749571,1.22479141349591,6.10347257915889));
#2941=CARTESIAN_POINT('Ctrl Pts',(-12.0734015567445,1.24876937750648,6.09855205886143));
#2942=CARTESIAN_POINT('Ctrl Pts',(-12.2338521859541,1.28348145043716,6.09134419637203));
#2943=CARTESIAN_POINT('Ctrl Pts',(-12.3189795113601,1.2937973652787,6.08913440512663));
#2944=CARTESIAN_POINT('Ctrl Pts',(-12.4739508140748,1.29713192273053,6.08842485041812));
#2945=CARTESIAN_POINT('Ctrl Pts',(-12.5551051454825,1.29286923752959,6.08935069297525));
#2946=CARTESIAN_POINT('Ctrl Pts',(-12.7295007065038,1.26380109840075,6.095447288475));
#2947=CARTESIAN_POINT('Ctrl Pts',(-12.8129106573291,1.2417464539227,6.10003761945498));
#2948=CARTESIAN_POINT('Ctrl Pts',(-12.930645922683,1.19760572832424,6.10879842776981));
#2949=CARTESIAN_POINT('Ctrl Pts',(-12.967672799061,1.18158636714795,6.11192618102656));
#2950=CARTESIAN_POINT('Ctrl Pts',(-13.0777680399706,1.12775712925574,6.12217182297329));
#2951=CARTESIAN_POINT('Ctrl Pts',(-13.1487493610343,1.08425780301533,6.13011818982353));
#2952=CARTESIAN_POINT('Ctrl Pts',(-13.3056808909995,0.96681927406719,6.14991898018366));
#2953=CARTESIAN_POINT('Ctrl Pts',(-13.3666667789338,0.902791579314907,6.15937339329189));
#2954=CARTESIAN_POINT('Ctrl Pts',(-13.4542585130877,0.80419692839569,6.17320967835681));
#2955=CARTESIAN_POINT('Ctrl Pts',(-13.5029326073056,0.737209443905024,6.18166348309254));
#2956=CARTESIAN_POINT('Ctrl Pts',(-13.6075063036529,0.562364326693226,6.20050846236433));
#2957=CARTESIAN_POINT('Ctrl Pts',(-13.6532128199648,0.454665015701439,6.20944139197031));
#2958=CARTESIAN_POINT('Ctrl Pts',(-13.714760512167,0.231511174842811,6.2217703969669));
#2959=CARTESIAN_POINT('Ctrl Pts',(-13.7301962062682,0.116227382741286,6.22506783214625));
#2960=CARTESIAN_POINT('Ctrl Pts',(-13.730193598416,-1.52223171728111E-5,
6.22506754789523));
#2961=CARTESIAN_POINT('Ctrl Pts',(-13.7301935984159,-1.52267580922841E-5,
6.22506754789522));
#2962=CARTESIAN_POINT('Ctrl Pts',(-13.7301907271263,-0.12798100776143,6.22506723488593));
#2963=CARTESIAN_POINT('Ctrl Pts',(-13.7114805449995,-0.254640288623575,
6.22106154775522));
#2964=CARTESIAN_POINT('Ctrl Pts',(-13.6298980591205,-0.521908165468462,
6.2048534383784));
#2965=CARTESIAN_POINT('Ctrl Pts',(-13.5662496906304,-0.638614514310813,
6.19285613210405));
#2966=CARTESIAN_POINT('Ctrl Pts',(-13.4423944644575,-0.823037393434848,
6.17118502256686));
#2967=CARTESIAN_POINT('Ctrl Pts',(-13.3812304072417,-0.886826703639457,
6.16165378610988));
#2968=CARTESIAN_POINT('Ctrl Pts',(-13.2327372610965,-1.0337673323202,6.13975300469276));
#2969=CARTESIAN_POINT('Ctrl Pts',(-13.0886106045117,-1.12971057779523,6.12204728865717));
#2970=CARTESIAN_POINT('Ctrl Pts',(-12.8545066464152,-1.22726329564512,6.1029881561482));
#2971=CARTESIAN_POINT('Ctrl Pts',(-12.7697676836191,-1.25257942206277,6.09777084115763));
#2972=CARTESIAN_POINT('Ctrl Pts',(-12.6009891820413,-1.28598916676046,6.09081125870397));
#2973=CARTESIAN_POINT('Ctrl Pts',(-12.5151371030402,-1.29485665783831,6.08890895085005));
#2974=CARTESIAN_POINT('Ctrl Pts',(-12.4302293937643,-1.29485665783831,6.08890895085005));
#2975=CARTESIAN_POINT('Origin',(-12.4302293937643,0.,0.));
#2976=CARTESIAN_POINT('',(-10.7808324711337,-7.62350904702874E-16,6.22506754791384));
#2977=CARTESIAN_POINT('Origin',(-10.7808324711337,0.,0.));
#2978=CARTESIAN_POINT('',(-12.4302293937643,-7.62350904702875E-16,6.22506754791384));
#2979=CARTESIAN_POINT('',(-14.0796263163949,-7.62350904702874E-16,6.22506754791384));
#2980=CARTESIAN_POINT('',(-12.4302293937643,-7.62350904702875E-16,6.22506754791384));
#2981=CARTESIAN_POINT('Origin',(-14.0796263163949,0.,0.));
#2982=CARTESIAN_POINT('',(-12.4302293937643,6.08890895085005,1.29485665783831));
#2983=CARTESIAN_POINT('Ctrl Pts',(-12.4302293937643,6.08890895085005,1.29485665783831));
#2984=CARTESIAN_POINT('Ctrl Pts',(-12.3718488355339,6.08890895085005,1.29485665783831));
#2985=CARTESIAN_POINT('Ctrl Pts',(-12.3121124409535,6.0897882543227,1.29074255777323));
#2986=CARTESIAN_POINT('Ctrl Pts',(-12.2521561327521,6.09152855044746,1.28247646963738));
#2987=CARTESIAN_POINT('Ctrl Pts',(-12.1926670476362,6.09325528492125,1.27427479686196));
#2988=CARTESIAN_POINT('Ctrl Pts',(-12.1329614629979,6.09582968006873,1.261985531925));
#2989=CARTESIAN_POINT('Ctrl Pts',(-12.0741489521671,6.09918373770257,1.24556160419089));
#2990=CARTESIAN_POINT('Ctrl Pts',(-12.0257014746808,6.10194668098466,1.23203220614457));
#2991=CARTESIAN_POINT('Ctrl Pts',(-11.9778600217895,6.10523781280487,1.21569687634397));
#2992=CARTESIAN_POINT('Ctrl Pts',(-11.9312448343282,6.10899291380237,1.19652478252752));
#2993=CARTESIAN_POINT('Ctrl Pts',(-11.8511268068043,6.11544684655385,1.16357349725477));
#2994=CARTESIAN_POINT('Ctrl Pts',(-11.7746166055436,6.12324782931237,1.12232382755702));
#2995=CARTESIAN_POINT('Ctrl Pts',(-11.7037724666101,6.13154545346576,1.07499596658472));
#2996=CARTESIAN_POINT('Ctrl Pts',(-11.6511399287433,6.13771004271806,1.03983447726073));
#2997=CARTESIAN_POINT('Ctrl Pts',(-11.6016347814191,6.14414724944668,1.00131822095112));
#2998=CARTESIAN_POINT('Ctrl Pts',(-11.556101032204,6.15054104774044,0.960370134973962));
#2999=CARTESIAN_POINT('Ctrl Pts',(-11.5403457122178,6.15275339220543,0.946201519199617));
#3000=CARTESIAN_POINT('Ctrl Pts',(-11.5250658709222,6.1549609506989,0.931741872426695));
#3001=CARTESIAN_POINT('Ctrl Pts',(-11.5102964728551,6.15715212281449,0.917029831909005));
#3002=CARTESIAN_POINT('Ctrl Pts',(-11.4670495554528,6.16356818926938,0.873950865643971));
#3003=CARTESIAN_POINT('Ctrl Pts',(-11.4259525115292,6.17018157540767,0.826420862407318));
#3004=CARTESIAN_POINT('Ctrl Pts',(-11.3879789718363,6.17658890898875,0.775380826076553));
#3005=CARTESIAN_POINT('Ctrl Pts',(-11.3545272206854,6.18223327425541,0.730418502103837));
#3006=CARTESIAN_POINT('Ctrl Pts',(-11.3234993860063,6.18771715669703,0.682732482406092));
#3007=CARTESIAN_POINT('Ctrl Pts',(-11.2955610590574,6.19280256866837,0.632978926651143));
#3008=CARTESIAN_POINT('Ctrl Pts',(-11.2709494590157,6.19728244055603,0.58914972323683));
#3009=CARTESIAN_POINT('Ctrl Pts',(-11.2487354118454,6.20145324377775,0.543716269066643));
#3010=CARTESIAN_POINT('Ctrl Pts',(-11.2293739328148,6.20518515020226,0.497135019687165));
#3011=CARTESIAN_POINT('Ctrl Pts',(-11.2095362147048,6.20900885125039,0.449407999817292));
#3012=CARTESIAN_POINT('Ctrl Pts',(-11.1926931212539,6.21237113545347,0.400470739216812));
#3013=CARTESIAN_POINT('Ctrl Pts',(-11.1788273455236,6.21517025603366,0.350891243271439));
#3014=CARTESIAN_POINT('Ctrl Pts',(-11.1650963685599,6.21794216443263,0.301793743792303));
#3015=CARTESIAN_POINT('Ctrl Pts',(-11.1542851015898,6.22016166015472,0.252066628203633));
#3016=CARTESIAN_POINT('Ctrl Pts',(-11.1463767375417,6.22178063693777,0.202266363778714));
#3017=CARTESIAN_POINT('Ctrl Pts',(-11.1384625687977,6.2234008020409,0.152429546232813));
#3018=CARTESIAN_POINT('Ctrl Pts',(-11.1334555659694,6.22441953396933,0.102519680035822));
#3019=CARTESIAN_POINT('Ctrl Pts',(-11.131338884949,6.22484110271258,0.0530963470502571));
#3020=CARTESIAN_POINT('Ctrl Pts',(-11.130569311005,6.22499437489543,0.0351272204211175));
#3021=CARTESIAN_POINT('Ctrl Pts',(-11.1301818010262,6.22506921164877,0.0172224098454036));
#3022=CARTESIAN_POINT('Ctrl Pts',(-11.1301755454826,6.22506751983931,-0.000591212059548435));
#3023=CARTESIAN_POINT('Ctrl Pts',(-11.1301632788032,6.22506420232037,-0.0355224674101873));
#3024=CARTESIAN_POINT('Ctrl Pts',(-11.131617028533,6.22477123151765,-0.0701045290928973));
#3025=CARTESIAN_POINT('Ctrl Pts',(-11.1345194766772,6.22418013883881,-0.105107446807877));
#3026=CARTESIAN_POINT('Ctrl Pts',(-11.135048849963,6.22407233030683,-0.111491577941726));
#3027=CARTESIAN_POINT('Ctrl Pts',(-11.1356264150422,6.2239544651859,-0.117889707248624));
#3028=CARTESIAN_POINT('Ctrl Pts',(-11.1362520668421,6.22382630456588,-0.124306502983067));
#3029=CARTESIAN_POINT('Ctrl Pts',(-11.1398494021155,6.22308941430334,-0.161201411048983));
#3030=CARTESIAN_POINT('Ctrl Pts',(-11.1450364608977,6.22200768798106,-0.198712719075032));
#3031=CARTESIAN_POINT('Ctrl Pts',(-11.1519002434474,6.2205883070516,-0.236108217271136));
#3032=CARTESIAN_POINT('Ctrl Pts',(-11.1527753381609,6.22040734375055,-0.240875938647017));
#3033=CARTESIAN_POINT('Ctrl Pts',(-11.1536776877754,6.22022096151269,-0.24564177918353));
#3034=CARTESIAN_POINT('Ctrl Pts',(-11.1546074725907,6.22002923635036,-0.250404223280646));
#3035=CARTESIAN_POINT('Ctrl Pts',(-11.1647679800375,6.21793410110223,-0.302447285201551));
#3036=CARTESIAN_POINT('Ctrl Pts',(-11.1782047149051,6.21519654817054,-0.354085778689705));
#3037=CARTESIAN_POINT('Ctrl Pts',(-11.1948269593364,6.21189458999722,-0.404761138022572));
#3038=CARTESIAN_POINT('Ctrl Pts',(-11.2051082660968,6.20985223975804,-0.436105215331061));
#3039=CARTESIAN_POINT('Ctrl Pts',(-11.2166082711959,6.20759503999576,-0.467080908070465));
#3040=CARTESIAN_POINT('Ctrl Pts',(-11.229305507763,6.20515130840228,-0.497557248890469));
#3041=CARTESIAN_POINT('Ctrl Pts',(-11.2511175385676,6.20095332811627,-0.549911230110713));
#3042=CARTESIAN_POINT('Ctrl Pts',(-11.2764626366353,6.19620164677118,-0.600795969759021));
#3043=CARTESIAN_POINT('Ctrl Pts',(-11.3047450780971,6.1910847502828,-0.649565694064773));
#3044=CARTESIAN_POINT('Ctrl Pts',(-11.3362202928213,6.18539021305868,-0.703840978135764));
#3045=CARTESIAN_POINT('Ctrl Pts',(-11.371333470988,6.17924349051508,-0.755496412322283));
#3046=CARTESIAN_POINT('Ctrl Pts',(-11.409263504348,6.17297318268182,-0.803659170283709));
#3047=CARTESIAN_POINT('Ctrl Pts',(-11.4410840719414,6.16771284577818,-0.844064257214491));
#3048=CARTESIAN_POINT('Ctrl Pts',(-11.4748871428235,6.16236744413282,-0.882011602979711));
#3049=CARTESIAN_POINT('Ctrl Pts',(-11.5101879037145,6.15715725915592,-0.916995344652119));
#3050=CARTESIAN_POINT('Ctrl Pts',(-11.5373386303507,6.15314997136772,-0.943902243622234));
#3051=CARTESIAN_POINT('Ctrl Pts',(-11.5659110990122,6.14899975657276,-0.970528187457023));
#3052=CARTESIAN_POINT('Ctrl Pts',(-11.5960932344668,6.14489940158615,-0.995829965644821));
#3053=CARTESIAN_POINT('Ctrl Pts',(-11.5979244007967,6.1446506308521,-0.997365038084425));
#3054=CARTESIAN_POINT('Ctrl Pts',(-11.5997614921715,6.14440205919207,-0.998895239088563));
#3055=CARTESIAN_POINT('Ctrl Pts',(-11.6016045505592,6.14415373553954,-1.00042033673129));
#3056=CARTESIAN_POINT('Ctrl Pts',(-11.6615724669768,6.13607398497985,-1.05004270820941));
#3057=CARTESIAN_POINT('Ctrl Pts',(-11.7278574681358,6.12825826776771,-1.09426801163532));
#3058=CARTESIAN_POINT('Ctrl Pts',(-11.7982730880567,6.12119892536502,-1.13242646216));
#3059=CARTESIAN_POINT('Ctrl Pts',(-11.8606994828957,6.11494052280277,-1.16625552596115));
#3060=CARTESIAN_POINT('Ctrl Pts',(-11.9263723642927,6.10927767330432,-1.19531701975332));
#3061=CARTESIAN_POINT('Ctrl Pts',(-11.993768239231,6.10451864249069,-1.2191464717472));
#3062=CARTESIAN_POINT('Ctrl Pts',(-12.0559835126778,6.10012542994343,-1.24114419598842));
#3063=CARTESIAN_POINT('Ctrl Pts',(-12.1196670734389,6.09650308785304,-1.25868370635078));
#3064=CARTESIAN_POINT('Ctrl Pts',(-12.1836204393827,6.09385116522343,-1.27139449117692));
#3065=CARTESIAN_POINT('Ctrl Pts',(-12.2424548053251,6.09141150963786,-1.28308787048294));
#3066=CARTESIAN_POINT('Ctrl Pts',(-12.3015175131772,6.08979341584715,-1.2906947703834));
#3067=CARTESIAN_POINT('Ctrl Pts',(-12.359875449219,6.08910837609838,-1.29391852920443));
#3068=CARTESIAN_POINT('Ctrl Pts',(-12.3833869081744,6.08883238477606,-1.29521732896233));
#3069=CARTESIAN_POINT('Ctrl Pts',(-12.4067839719209,6.088707294906,-1.29580456658866));
#3070=CARTESIAN_POINT('Ctrl Pts',(-12.4300056202704,6.08873798595888,-1.29566033914429));
#3071=CARTESIAN_POINT('Ctrl Pts',(-12.4891266282453,6.08881612364982,-1.29529314419929));
#3072=CARTESIAN_POINT('Ctrl Pts',(-12.5495196242162,6.08974550575461,-1.29094567075297));
#3073=CARTESIAN_POINT('Ctrl Pts',(-12.6100740656419,6.0915305368075,-1.28246703475439));
#3074=CARTESIAN_POINT('Ctrl Pts',(-12.6686715853072,6.09325788148715,-1.27426240057785));
#3075=CARTESIAN_POINT('Ctrl Pts',(-12.7274202842567,6.09578656737953,-1.26218925802848));
#3076=CARTESIAN_POINT('Ctrl Pts',(-12.7853138452971,6.09907347136525,-1.24610142724366));
#3077=CARTESIAN_POINT('Ctrl Pts',(-12.8340958169417,6.10184306532609,-1.2325455828447));
#3078=CARTESIAN_POINT('Ctrl Pts',(-12.8822706409192,6.10515031552918,-1.21613912550678));
#3079=CARTESIAN_POINT('Ctrl Pts',(-12.9292362816626,6.10894103006689,-1.19678965037943));
#3080=CARTESIAN_POINT('Ctrl Pts',(-13.0093877866196,6.1154102588531,-1.16376785983131));
#3081=CARTESIAN_POINT('Ctrl Pts',(-13.0859056680526,6.12321644231893,-1.12249606627535));
#3082=CARTESIAN_POINT('Ctrl Pts',(-13.1567588548687,6.13151928842058,-1.07514519569055));
#3083=CARTESIAN_POINT('Ctrl Pts',(-13.2098424175907,6.13773982233885,-1.03966968609699));
#3084=CARTESIAN_POINT('Ctrl Pts',(-13.2597463410517,6.1442375291199,-1.00078201446416));
#3085=CARTESIAN_POINT('Ctrl Pts',(-13.3056164890128,6.15069123844581,-0.959407768050671));
#3086=CARTESIAN_POINT('Ctrl Pts',(-13.3209714359044,6.15285160566409,-0.945557815857451));
#3087=CARTESIAN_POINT('Ctrl Pts',(-13.3358743727583,6.15500743188913,-0.931429344163949));
#3088=CARTESIAN_POINT('Ctrl Pts',(-13.3502932603732,6.15714801078641,-0.91705744059957));
#3089=CARTESIAN_POINT('Ctrl Pts',(-13.395064219943,6.16379455480738,-0.872432367528252));
#3090=CARTESIAN_POINT('Ctrl Pts',(-13.4374769917471,6.17063459464968,-0.823155456071043));
#3091=CARTESIAN_POINT('Ctrl Pts',(-13.4764946351208,6.17723981039304,-0.770178096926561));
#3092=CARTESIAN_POINT('Ctrl Pts',(-13.5106703929134,6.18302535339088,-0.723774951116996));
#3093=CARTESIAN_POINT('Ctrl Pts',(-13.5422413743335,6.18863012393773,-0.674532981746127));
#3094=CARTESIAN_POINT('Ctrl Pts',(-13.5705107519144,6.19380382459731,-0.623105254747394));
#3095=CARTESIAN_POINT('Ctrl Pts',(-13.5928556619771,6.19789326291618,-0.5824553348391));
#3096=CARTESIAN_POINT('Ctrl Pts',(-13.6131378073445,6.20171394782517,-0.540440088961139));
#3097=CARTESIAN_POINT('Ctrl Pts',(-13.6310130660832,6.20516488928487,-0.497387849546377));
#3098=CARTESIAN_POINT('Ctrl Pts',(-13.65008358127,6.20884658321043,-0.451456856457475));
#3099=CARTESIAN_POINT('Ctrl Pts',(-13.6664145680264,6.21210579699621,-0.404341033695851));
#3100=CARTESIAN_POINT('Ctrl Pts',(-13.6800047881991,6.21484377769198,-0.356626968937239));
#3101=CARTESIAN_POINT('Ctrl Pts',(-13.693474517426,6.21755748344005,-0.309335937265786));
#3102=CARTESIAN_POINT('Ctrl Pts',(-13.7042518639233,6.21975901285525,-0.261457409881135));
#3103=CARTESIAN_POINT('Ctrl Pts',(-13.7123356221791,6.22140298052968,-0.213567155589214));
#3104=CARTESIAN_POINT('Ctrl Pts',(-13.7204483419628,6.22305283801602,-0.165505325788445));
#3105=CARTESIAN_POINT('Ctrl Pts',(-13.725848138396,6.22414109616072,-0.117431885941534));
#3106=CARTESIAN_POINT('Ctrl Pts',(-13.7285337929633,6.22467474546693,-0.0699306030019548));
#3107=CARTESIAN_POINT('Ctrl Pts',(-13.7298600330228,6.22493827417842,-0.0464733404489176));
#3108=CARTESIAN_POINT('Ctrl Pts',(-13.730524397251,6.22506737084474,-0.0231556133287919));
#3109=CARTESIAN_POINT('Ctrl Pts',(-13.7305267389083,6.22506754773146,-4.7651618804912E-5));
#3110=CARTESIAN_POINT('Ctrl Pts',(-13.7305314774732,6.22506790567845,0.0467134926687206));
#3111=CARTESIAN_POINT('Ctrl Pts',(-13.7278223185331,6.22453713191487,0.0943326037746073));
#3112=CARTESIAN_POINT('Ctrl Pts',(-13.7224017682409,6.22344254907136,0.142228036962457));
#3113=CARTESIAN_POINT('Ctrl Pts',(-13.7169997749408,6.22235171347937,0.189959502447259));
#3114=CARTESIAN_POINT('Ctrl Pts',(-13.7089049231458,6.22070084980274,0.237965202300239));
#3115=CARTESIAN_POINT('Ctrl Pts',(-13.6981196933575,6.2185093699227,0.285669725861333));
#3116=CARTESIAN_POINT('Ctrl Pts',(-13.6872081374435,6.21629222149702,0.333933006886285));
#3117=CARTESIAN_POINT('Ctrl Pts',(-13.673542810278,6.21352173111101,0.381887809531659));
#3118=CARTESIAN_POINT('Ctrl Pts',(-13.6571262805493,6.21027173645692,0.428941645744985));
#3119=CARTESIAN_POINT('Ctrl Pts',(-13.649095512483,6.2086818783252,0.451959814109667));
#3120=CARTESIAN_POINT('Ctrl Pts',(-13.6404063683738,6.2069780829424,0.474762447833064));
#3121=CARTESIAN_POINT('Ctrl Pts',(-13.6310591489254,6.20517347780729,0.49728069176982));
#3122=CARTESIAN_POINT('Ctrl Pts',(-13.60875708102,6.20086776673589,0.551008263713592));
#3123=CARTESIAN_POINT('Ctrl Pts',(-13.5827087264517,6.19598442403786,0.603122184572173));
#3124=CARTESIAN_POINT('Ctrl Pts',(-13.5535786727981,6.1907256556975,0.652979197202176));
#3125=CARTESIAN_POINT('Ctrl Pts',(-13.5210316541874,6.18485003208627,0.708684453953247));
#3126=CARTESIAN_POINT('Ctrl Pts',(-13.4846375656099,6.17850594605293,0.761571903553669));
#3127=CARTESIAN_POINT('Ctrl Pts',(-13.445323369218,6.17204418421574,0.810762951903158));
#3128=CARTESIAN_POINT('Ctrl Pts',(-13.4152322050363,6.16709833884205,0.848413878235033));
#3129=CARTESIAN_POINT('Ctrl Pts',(-13.3834303242871,6.16208535244838,0.883899768089104));
#3130=CARTESIAN_POINT('Ctrl Pts',(-13.3503333798219,6.15718128343761,0.916834019316256));
#3131=CARTESIAN_POINT('Ctrl Pts',(-13.3074383542668,6.15082540470197,0.959518187624141));
#3132=CARTESIAN_POINT('Ctrl Pts',(-13.260254465564,6.14432948438849,1.00006283592689));
#3133=CARTESIAN_POINT('Ctrl Pts',(-13.2096360642912,6.13799486435182,1.03753796136853));
#3134=CARTESIAN_POINT('Ctrl Pts',(-13.1474956494906,6.13021832643703,1.08354336219305));
#3135=CARTESIAN_POINT('Ctrl Pts',(-13.0801792074,6.12268637557024,1.12492259137719));
#3136=CARTESIAN_POINT('Ctrl Pts',(-13.0092673791852,6.11603709544722,1.15998113053774));
#3137=CARTESIAN_POINT('Ctrl Pts',(-12.9830238921301,6.11357628881979,1.17295581109232));
#3138=CARTESIAN_POINT('Ctrl Pts',(-12.9562879674199,6.11123687837181,1.18506500914902));
#3139=CARTESIAN_POINT('Ctrl Pts',(-12.9291397252248,6.10905193800453,1.19622338835736));
#3140=CARTESIAN_POINT('Ctrl Pts',(-12.8721572340207,6.10446588251095,1.21964414026165));
#3141=CARTESIAN_POINT('Ctrl Pts',(-12.8133582604497,6.1005650066165,1.23887411122538));
#3142=CARTESIAN_POINT('Ctrl Pts',(-12.7538653798013,6.09746733340917,1.2539370375334));
#3143=CARTESIAN_POINT('Ctrl Pts',(-12.6943518161327,6.09436858327908,1.26900520054885));
#3144=CARTESIAN_POINT('Ctrl Pts',(-12.6341438628219,6.09207357027527,1.27990354745453));
#3145=CARTESIAN_POINT('Ctrl Pts',(-12.5743652663738,6.09064906637895,1.28664677604512));
#3146=CARTESIAN_POINT('Ctrl Pts',(-12.5258366133329,6.08949264485941,1.2921209728328));
#3147=CARTESIAN_POINT('Ctrl Pts',(-12.4775909192552,6.08890895085005,1.29485665783831));
#3148=CARTESIAN_POINT('Ctrl Pts',(-12.4302293937643,6.08890895085005,1.29485665783831));
#3149=CARTESIAN_POINT('',(-12.4302293937643,-6.08890895085005,-1.29485665783831));
#3150=CARTESIAN_POINT('Ctrl Pts',(-12.4302293937643,-6.08890895085005,-1.29485665783831));
#3151=CARTESIAN_POINT('Ctrl Pts',(-12.3719064521781,-6.08890895085005,-1.29485665783831));
#3152=CARTESIAN_POINT('Ctrl Pts',(-12.3122256701442,-6.08979172951493,-1.29072628612679));
#3153=CARTESIAN_POINT('Ctrl Pts',(-12.2523216952069,-6.09153589587755,-1.28244157969294));
#3154=CARTESIAN_POINT('Ctrl Pts',(-12.1926889042377,-6.09327216643767,-1.27419437794166));
#3155=CARTESIAN_POINT('Ctrl Pts',(-12.1328349365697,-6.09586206915765,-1.261830303888));
#3156=CARTESIAN_POINT('Ctrl Pts',(-12.0738790998279,-6.09923397540106,-1.24531557823849));
#3157=CARTESIAN_POINT('Ctrl Pts',(-12.0255019130074,-6.10200084883197,-1.23176414699457));
#3158=CARTESIAN_POINT('Ctrl Pts',(-11.9777294641826,-6.10529336450592,-1.21541773500516));
#3159=CARTESIAN_POINT('Ctrl Pts',(-11.9311801838106,-6.10904609419394,-1.19625323201392));
#3160=CARTESIAN_POINT('Ctrl Pts',(-11.8510483344045,-6.11550619771905,-1.16326266684596));
#3161=CARTESIAN_POINT('Ctrl Pts',(-11.7745451807163,-6.12331490566863,-1.12196034321072));
#3162=CARTESIAN_POINT('Ctrl Pts',(-11.7036935021763,-6.13161948888405,-1.07457359898116));
#3163=CARTESIAN_POINT('Ctrl Pts',(-11.6511301610919,-6.13778048110204,-1.03941838951899));
#3164=CARTESIAN_POINT('Ctrl Pts',(-11.6016773003432,-6.1442129054961,-1.00091451711278));
#3165=CARTESIAN_POINT('Ctrl Pts',(-11.5561608570514,-6.15060133425726,-0.959983959825811));
#3166=CARTESIAN_POINT('Ctrl Pts',(-11.5403243432848,-6.15282405713949,-0.945743011125359));
#3167=CARTESIAN_POINT('Ctrl Pts',(-11.5249643523102,-6.15504186893641,-0.931208422868594));
#3168=CARTESIAN_POINT('Ctrl Pts',(-11.5101156714317,-6.15724300247758,-0.916419437010658));
#3169=CARTESIAN_POINT('Ctrl Pts',(-11.4645711583886,-6.16399441400674,-0.871058023103533));
#3170=CARTESIAN_POINT('Ctrl Pts',(-11.4214166133875,-6.17094128665832,-0.820917691856838));
#3171=CARTESIAN_POINT('Ctrl Pts',(-11.3817855353081,-6.17764011919321,-0.766960581662782));
#3172=CARTESIAN_POINT('Ctrl Pts',(-11.3472092195376,-6.18348454635098,-0.719885453492252));
#3173=CARTESIAN_POINT('Ctrl Pts',(-11.3153148857571,-6.1891395359759,-0.669905289238284));
#3174=CARTESIAN_POINT('Ctrl Pts',(-11.2868552819188,-6.19434788918216,-0.617673217708659));
#3175=CARTESIAN_POINT('Ctrl Pts',(-11.2655337998714,-6.19824990447424,-0.578541781384198));
#3176=CARTESIAN_POINT('Ctrl Pts',(-11.2461401519929,-6.2019019101112,-0.538146702804389));
#3177=CARTESIAN_POINT('Ctrl Pts',(-11.2289908685175,-6.20521457200396,-0.496767643350301));
#3178=CARTESIAN_POINT('Ctrl Pts',(-11.2095257717429,-6.20897457074771,-0.449800818300852));
#3179=CARTESIAN_POINT('Ctrl Pts',(-11.1929798364322,-6.21228724335781,-0.401664913240023));
#3180=CARTESIAN_POINT('Ctrl Pts',(-11.1793139172197,-6.21505410315874,-0.352942588673756));
#3181=CARTESIAN_POINT('Ctrl Pts',(-11.1658161850305,-6.21778691110363,-0.304819891736394));
#3182=CARTESIAN_POINT('Ctrl Pts',(-11.1551280162058,-6.21998715159152,-0.256125313797636));
#3183=CARTESIAN_POINT('Ctrl Pts',(-11.1472116929566,-6.22161079510395,-0.207424902882935));
#3184=CARTESIAN_POINT('Ctrl Pts',(-11.142675300804,-6.22254121235152,-0.179517482361168));
#3185=CARTESIAN_POINT('Ctrl Pts',(-11.1390491219431,-6.22328324189245,-0.151608217023861));
#3186=CARTESIAN_POINT('Ctrl Pts',(-11.1363260588406,-6.22383632196961,-0.1238039313667));
#3187=CARTESIAN_POINT('Ctrl Pts',(-11.1301829852291,-6.22508403878672,-0.0610790634233799));
#3188=CARTESIAN_POINT('Ctrl Pts',(-11.128636117224,-6.22537741498978,0.00111173707387613));
#3189=CARTESIAN_POINT('Ctrl Pts',(-11.1317392028041,-6.22474640435053,0.0632311443445715));
#3190=CARTESIAN_POINT('Ctrl Pts',(-11.1348422883842,-6.22411539371129,0.125350551615267));
#3191=CARTESIAN_POINT('Ctrl Pts',(-11.1425953275496,-6.22255997486812,0.187398858806157));
#3192=CARTESIAN_POINT('Ctrl Pts',(-11.155052068279,-6.22005198588599,0.249838485757963));
#3193=CARTESIAN_POINT('Ctrl Pts',(-11.1636782663859,-6.21831522261222,0.293077451993458));
#3194=CARTESIAN_POINT('Ctrl Pts',(-11.1745601043725,-6.21611498744589,0.336503678440918));
#3195=CARTESIAN_POINT('Ctrl Pts',(-11.1876619822991,-6.21348992882496,0.379485020100749));
#3196=CARTESIAN_POINT('Ctrl Pts',(-11.2009499746653,-6.21082758079276,0.423076919145163));
#3197=CARTESIAN_POINT('Ctrl Pts',(-11.2165215270484,-6.20772831978472,0.466211022440592));
#3198=CARTESIAN_POINT('Ctrl Pts',(-11.2343395007458,-6.20428609450448,0.508232263466642));
#3199=CARTESIAN_POINT('Ctrl Pts',(-11.2370078547666,-6.20377059954286,0.514525209530911));
#3200=CARTESIAN_POINT('Ctrl Pts',(-11.2397265891724,-6.20324750754818,0.520793208244316));
#3201=CARTESIAN_POINT('Ctrl Pts',(-11.2424955792299,-6.20271723227493,0.527034071507458));
#3202=CARTESIAN_POINT('Ctrl Pts',(-11.2689548168362,-6.19765015757953,0.586668985509251));
#3203=CARTESIAN_POINT('Ctrl Pts',(-11.3000028295008,-6.19192219217637,0.643833523819529));
#3204=CARTESIAN_POINT('Ctrl Pts',(-11.3346739550651,-6.1858270830772,0.697860497777764));
#3205=CARTESIAN_POINT('Ctrl Pts',(-11.3746009810791,-6.17880799801434,0.760077583597297));
#3206=CARTESIAN_POINT('Ctrl Pts',(-11.4193328579437,-6.17130282806334,0.818133275908099));
#3207=CARTESIAN_POINT('Ctrl Pts',(-11.4673948225036,-6.16382680012626,0.871036827083257));
#3208=CARTESIAN_POINT('Ctrl Pts',(-11.4814127796881,-6.1616463099925,0.886466902030723));
#3209=CARTESIAN_POINT('Ctrl Pts',(-11.495714020902,-6.15946861786056,0.901458876654718));
#3210=CARTESIAN_POINT('Ctrl Pts',(-11.5102619553448,-6.15730711289799,0.915988588108959));
#3211=CARTESIAN_POINT('Ctrl Pts',(-11.5532785793428,-6.15091578314529,0.958951328756652));
#3212=CARTESIAN_POINT('Ctrl Pts',(-11.6006222582692,-6.14438414393611,0.99973456931751));
#3213=CARTESIAN_POINT('Ctrl Pts',(-11.6514306134181,-6.13801702466402,1.03740685414387));
#3214=CARTESIAN_POINT('Ctrl Pts',(-11.7142249038981,-6.13014787133441,1.08396621213724));
#3215=CARTESIAN_POINT('Ctrl Pts',(-11.7823113511379,-6.12253156578081,1.12577348439782));
#3216=CARTESIAN_POINT('Ctrl Pts',(-11.8540619600466,-6.1158253205787,1.16109716400415));
#3217=CARTESIAN_POINT('Ctrl Pts',(-11.8793592205985,-6.11346088584032,1.1735513067668));
#3218=CARTESIAN_POINT('Ctrl Pts',(-11.905111962326,-6.11121002907956,1.18519970187327));
#3219=CARTESIAN_POINT('Ctrl Pts',(-11.9312488347654,-6.10910214646688,1.19596694775559));
#3220=CARTESIAN_POINT('Ctrl Pts',(-11.9878698013094,-6.10453578715331,1.21929230431032));
#3221=CARTESIAN_POINT('Ctrl Pts',(-12.0462941969317,-6.10065260800729,1.23844210513609));
#3222=CARTESIAN_POINT('Ctrl Pts',(-12.1054170485769,-6.0975651052557,1.2534615124758));
#3223=CARTESIAN_POINT('Ctrl Pts',(-12.1648706860128,-6.09446032826901,1.26856495173198));
#3224=CARTESIAN_POINT('Ctrl Pts',(-12.2250306169031,-6.09216011743502,1.27949177271444));
#3225=CARTESIAN_POINT('Ctrl Pts',(-12.2847732176283,-6.09072680961869,1.28627870490117));
#3226=CARTESIAN_POINT('Ctrl Pts',(-12.3337654636889,-6.08955141771465,1.29184436571359));
#3227=CARTESIAN_POINT('Ctrl Pts',(-12.3824770589856,-6.08895803534379,1.29462582241761));
#3228=CARTESIAN_POINT('Ctrl Pts',(-12.4302883476924,-6.08895542042789,1.29463812091715));
#3229=CARTESIAN_POINT('Ctrl Pts',(-12.4886595445203,-6.08895222796488,1.29465313574223));
#3230=CARTESIAN_POINT('Ctrl Pts',(-12.5483726894007,-6.08982955021465,1.29054765466148));
#3231=CARTESIAN_POINT('Ctrl Pts',(-12.6083004626829,-6.09156796607547,1.28228923834413));
#3232=CARTESIAN_POINT('Ctrl Pts',(-12.667837119946,-6.0932950362404,1.27408472022353));
#3233=CARTESIAN_POINT('Ctrl Pts',(-12.7275856132271,-6.09587202812029,1.2617812342542));
#3234=CARTESIAN_POINT('Ctrl Pts',(-12.7864405513443,-6.09922962602741,1.24533688015717));
#3235=CARTESIAN_POINT('Ctrl Pts',(-12.8348827488882,-6.10199319058618,1.23180189609072));
#3236=CARTESIAN_POINT('Ctrl Pts',(-12.8827196010596,-6.10528469631702,1.21546142914907));
#3237=CARTESIAN_POINT('Ctrl Pts',(-12.9293347417047,-6.10903936174148,1.19628761290221));
#3238=CARTESIAN_POINT('Ctrl Pts',(-13.0094634914978,-6.1154934159863,1.16332892387194));
#3239=CARTESIAN_POINT('Ctrl Pts',(-13.0859749662094,-6.12329203356386,1.12208290179085));
#3240=CARTESIAN_POINT('Ctrl Pts',(-13.1568259029017,-6.13158884944212,1.07474841590352));
#3241=CARTESIAN_POINT('Ctrl Pts',(-13.2096726789799,-6.13777733461041,1.0394422492776));
#3242=CARTESIAN_POINT('Ctrl Pts',(-13.2593702313246,-6.1442414248502,1.00074886802867));
#3243=CARTESIAN_POINT('Ctrl Pts',(-13.3050706631998,-6.15066229423468,0.959593308839638));
#3244=CARTESIAN_POINT('Ctrl Pts',(-13.320640163871,-6.1528497950107,0.945572182996293));
#3245=CARTESIAN_POINT('Ctrl Pts',(-13.3357457307592,-6.15503267991332,0.931265399040215));
#3246=CARTESIAN_POINT('Ctrl Pts',(-13.3503538359836,-6.15719976089305,0.916709921702932));
#3247=CARTESIAN_POINT('Ctrl Pts',(-13.3951327134421,-6.16384261101928,0.872092366857553));
#3248=CARTESIAN_POINT('Ctrl Pts',(-13.4375529670986,-6.17067969598177,0.822817425220914));
#3249=CARTESIAN_POINT('Ctrl Pts',(-13.4765765828874,-6.17728224695273,0.769837656634619));
#3250=CARTESIAN_POINT('Ctrl Pts',(-13.5107493178741,-6.18306405932469,0.723443606392037));
#3251=CARTESIAN_POINT('Ctrl Pts',(-13.5423173768509,-6.18866540771235,0.674208745551412));
#3252=CARTESIAN_POINT('Ctrl Pts',(-13.5705837162355,-6.19383588730143,0.622786462013254));
#3253=CARTESIAN_POINT('Ctrl Pts',(-13.5929149547238,-6.19792071806891,0.582161347396281));
#3254=CARTESIAN_POINT('Ctrl Pts',(-13.6131854367614,-6.20173719344176,0.540171244993376));
#3255=CARTESIAN_POINT('Ctrl Pts',(-13.6310514543373,-6.20518441878562,0.497144149065676));
#3256=CARTESIAN_POINT('Ctrl Pts',(-13.6501118088316,-6.20886208991722,0.4512407070838));
#3257=CARTESIAN_POINT('Ctrl Pts',(-13.6664354784256,-6.21211785257913,0.404152460898107));
#3258=CARTESIAN_POINT('Ctrl Pts',(-13.6800210197033,-6.21485299465703,0.356466311020465));
#3259=CARTESIAN_POINT('Ctrl Pts',(-13.6934861915508,-6.2175639030672,0.309202665816666));
#3260=CARTESIAN_POINT('Ctrl Pts',(-13.7042615403867,-6.21976323071201,0.26135185013742));
#3261=CARTESIAN_POINT('Ctrl Pts',(-13.7123456608225,-6.22140563057677,0.213489943364428));
#3262=CARTESIAN_POINT('Ctrl Pts',(-13.720459026399,-6.22305397199268,0.165454891200063));
#3263=CARTESIAN_POINT('Ctrl Pts',(-13.7258616567617,-6.22414131346989,0.117408868488908));
#3264=CARTESIAN_POINT('Ctrl Pts',(-13.7285521312143,-6.22467468466975,0.0699360144815334));
#3265=CARTESIAN_POINT('Ctrl Pts',(-13.7298850723235,-6.22493893263467,0.0464165498699207));
#3266=CARTESIAN_POINT('Ctrl Pts',(-13.7305523130127,-6.22506802791389,0.0230377781326179));
#3267=CARTESIAN_POINT('Ctrl Pts',(-13.7305536805202,-6.22506754657021,-0.000129338362996957));
#3268=CARTESIAN_POINT('Ctrl Pts',(-13.7305564396758,-6.22506657538568,-0.04687254071794));
#3269=CARTESIAN_POINT('Ctrl Pts',(-13.7278463221129,-6.22453485270891,-0.0944754434099186));
#3270=CARTESIAN_POINT('Ctrl Pts',(-13.7224257748104,-6.22343961888028,-0.142356194952201));
#3271=CARTESIAN_POINT('Ctrl Pts',(-13.7170239399395,-6.22234816594072,-0.190071655937385));
#3272=CARTESIAN_POINT('Ctrl Pts',(-13.7089303565374,-6.22069701267219,-0.238062851811778));
#3273=CARTESIAN_POINT('Ctrl Pts',(-13.6981474463289,-6.2185054880869,-0.285754213832793));
#3274=CARTESIAN_POINT('Ctrl Pts',(-13.6872385727785,-6.2162883626429,-0.334002694778496));
#3275=CARTESIAN_POINT('Ctrl Pts',(-13.6735771732997,-6.21351817970532,-0.381944090359962));
#3276=CARTESIAN_POINT('Ctrl Pts',(-13.6571657554824,-6.21026868661577,-0.428985799449899));
#3277=CARTESIAN_POINT('Ctrl Pts',(-13.6491280918821,-6.2086772133734,-0.45202496870754));
#3278=CARTESIAN_POINT('Ctrl Pts',(-13.6404307942755,-6.20697158202696,-0.474848405373014));
#3279=CARTESIAN_POINT('Ctrl Pts',(-13.6310741572456,-6.20516495747886,-0.497386998791111));
#3280=CARTESIAN_POINT('Ctrl Pts',(-13.6087805380563,-6.20086039809872,-0.551088645774124));
#3281=CARTESIAN_POINT('Ctrl Pts',(-13.5827438257079,-6.19597875730673,-0.603178538196193));
#3282=CARTESIAN_POINT('Ctrl Pts',(-13.5536276272883,-6.19072206117842,-0.653013275001991));
#3283=CARTESIAN_POINT('Ctrl Pts',(-13.5210961880492,-6.18484877070857,-0.708693473667695));
#3284=CARTESIAN_POINT('Ctrl Pts',(-13.4847204648596,-6.17850748195645,-0.761558070337211));
#3285=CARTESIAN_POINT('Ctrl Pts',(-13.4454260438486,-6.17204874111248,-0.810728261146633));
#3286=CARTESIAN_POINT('Ctrl Pts',(-13.4153072475447,-6.1670981782882,-0.848416740149723));
#3287=CARTESIAN_POINT('Ctrl Pts',(-13.3834736943033,-6.16208041255199,-0.883935191456546));
#3288=CARTESIAN_POINT('Ctrl Pts',(-13.3503421930301,-6.15717216333953,-0.916895265058611));
#3289=CARTESIAN_POINT('Ctrl Pts',(-13.3074631907498,-6.15081987560474,-0.959552404542995));
#3290=CARTESIAN_POINT('Ctrl Pts',(-13.2602991426282,-6.14432752001126,-1.00007419215469));
#3291=CARTESIAN_POINT('Ctrl Pts',(-13.2097032383874,-6.13799606999591,-1.03753082884547));
#3292=CARTESIAN_POINT('Ctrl Pts',(-13.1476353114085,-6.13022903859053,-1.08348031479454));
#3293=CARTESIAN_POINT('Ctrl Pts',(-13.0804028303562,-6.12270564366612,-1.12481689112672));
#3294=CARTESIAN_POINT('Ctrl Pts',(-13.009580870276,-6.11606195335696,-1.15985005875305));
#3295=CARTESIAN_POINT('Ctrl Pts',(-12.9832375841035,-6.11359073348593,-1.17288116886729));
#3296=CARTESIAN_POINT('Ctrl Pts',(-12.9563976650894,-6.11124173558616,-1.18504037709756));
#3297=CARTESIAN_POINT('Ctrl Pts',(-12.9291421733597,-6.1090484410131,-1.19624124717609));
#3298=CARTESIAN_POINT('Ctrl Pts',(-12.8721614715127,-6.10446310953682,-1.21965793856075));
#3299=CARTESIAN_POINT('Ctrl Pts',(-12.8133644404388,-6.10056295946852,-1.2388841534509));
#3300=CARTESIAN_POINT('Ctrl Pts',(-12.7538735725762,-6.09746589322727,-1.2539440406255));
#3301=CARTESIAN_POINT('Ctrl Pts',(-12.694356022634,-6.09436743792968,-1.26901068226714));
#3302=CARTESIAN_POINT('Ctrl Pts',(-12.6341440133822,-6.09207276258628,-1.27990738444859));
#3303=CARTESIAN_POINT('Ctrl Pts',(-12.574361548274,-6.09064854118771,-1.28664926216048));
#3304=CARTESIAN_POINT('Ctrl Pts',(-12.5258340691386,-6.08949245178794,-1.29212187573379));
#3305=CARTESIAN_POINT('Ctrl Pts',(-12.47758962206,-6.08890895085005,-1.29485665783831));
#3306=CARTESIAN_POINT('Ctrl Pts',(-12.4302293937643,-6.08890895085005,-1.29485665783831));
#3307=CARTESIAN_POINT('',(-12.4302293937643,1.29485665783831,-6.08890895085005));
#3308=CARTESIAN_POINT('Ctrl Pts',(-12.4302293937643,1.29485665783831,-6.08890895085005));
#3309=CARTESIAN_POINT('Ctrl Pts',(-12.3719352419111,1.29485665783831,-6.08890895085005));
#3310=CARTESIAN_POINT('Ctrl Pts',(-12.3122852219887,1.29071977209828,-6.08979312075784));
#3311=CARTESIAN_POINT('Ctrl Pts',(-12.2524120064815,1.28242760146153,-6.09153883867612));
#3312=CARTESIAN_POINT('Ctrl Pts',(-12.1927308120721,1.27416202488182,-6.09327895785266));
#3313=CARTESIAN_POINT('Ctrl Pts',(-12.1328278514161,1.26176770689176,-6.09587512987746));
#3314=CARTESIAN_POINT('Ctrl Pts',(-12.0738249340326,1.24521625255819,-6.09925425445234));
#3315=CARTESIAN_POINT('Ctrl Pts',(-12.0254691329447,1.23165151933884,-6.10202361371524));
#3316=CARTESIAN_POINT('Ctrl Pts',(-11.9777178559071,1.21529437282654,-6.10531793806464));
#3317=CARTESIAN_POINT('Ctrl Pts',(-11.9311886135114,1.19612476042382,-6.10907124967381));
#3318=CARTESIAN_POINT('Ctrl Pts',(-11.8510584764837,1.16311189390145,-6.11553499930876));
#3319=CARTESIAN_POINT('Ctrl Pts',(-11.7745547714117,1.12179911546558,-6.12334463259387));
#3320=CARTESIAN_POINT('Ctrl Pts',(-11.703704178694,1.07438858878809,-6.13165190926328));
#3321=CARTESIAN_POINT('Ctrl Pts',(-11.6508998934495,1.03905396591142,-6.13784324500275));
#3322=CARTESIAN_POINT('Ctrl Pts',(-11.6012356756643,1.00033238611109,-6.14430943936365));
#3323=CARTESIAN_POINT('Ctrl Pts',(-11.5555505260111,0.959148077021043,-6.15073174040592));
#3324=CARTESIAN_POINT('Ctrl Pts',(-11.5399372428507,0.945072993882056,-6.15292661566572));
#3325=CARTESIAN_POINT('Ctrl Pts',(-11.52478871006,0.930710387099588,-6.15511676685479));
#3326=CARTESIAN_POINT('Ctrl Pts',(-11.5101384180024,0.916097539649635,-6.15729090379348));
#3327=CARTESIAN_POINT('Ctrl Pts',(-11.4598732878207,0.865960881860794,-6.16475036438488));
#3328=CARTESIAN_POINT('Ctrl Pts',(-11.4124955062379,0.81018432415652,-6.17241979163684));
#3329=CARTESIAN_POINT('Ctrl Pts',(-11.3695630860768,0.749809784999349,-6.17974524251682));
#3330=CARTESIAN_POINT('Ctrl Pts',(-11.3330563251016,0.698471452295889,-6.18597429933));
#3331=CARTESIAN_POINT('Ctrl Pts',(-11.2997638384491,0.643808791677128,-6.19195383145789));
#3332=CARTESIAN_POINT('Ctrl Pts',(-11.2706435584294,0.586479899545217,-6.1973790672767));
#3333=CARTESIAN_POINT('Ctrl Pts',(-11.2556374283266,0.556937435894595,-6.20017477509545));
#3334=CARTESIAN_POINT('Ctrl Pts',(-11.2417392277346,0.52668723531776,-6.20282398036088));
#3335=CARTESIAN_POINT('Ctrl Pts',(-11.2290800420475,0.495821129429846,-6.20529027392764));
#3336=CARTESIAN_POINT('Ctrl Pts',(-11.1986034220322,0.421511880498185,-6.21122780369755));
#3337=CARTESIAN_POINT('Ctrl Pts',(-11.1751084916239,0.34613055315122,-6.21590342372622));
#3338=CARTESIAN_POINT('Ctrl Pts',(-11.1586345171804,0.270072365609977,-6.21920629127414));
#3339=CARTESIAN_POINT('Ctrl Pts',(-11.1422659320947,0.194500746963393,-6.2224880293071));
#3340=CARTESIAN_POINT('Ctrl Pts',(-11.1328287596466,0.118261199967257,-6.22441440835855));
#3341=CARTESIAN_POINT('Ctrl Pts',(-11.1303615174059,0.0417484625205447,
-6.22492755315009));
#3342=CARTESIAN_POINT('Ctrl Pts',(-11.1279029777771,-0.0344943943881157,
-6.22543888794507));
#3343=CARTESIAN_POINT('Ctrl Pts',(-11.1323652855205,-0.111008206921567,
-6.22454690271329));
#3344=CARTESIAN_POINT('Ctrl Pts',(-11.1437865520568,-0.187399937894528,
-6.22224615708565));
#3345=CARTESIAN_POINT('Ctrl Pts',(-11.1469051234995,-0.208258664018226,
-6.22161793957682));
#3346=CARTESIAN_POINT('Ctrl Pts',(-11.1505425273872,-0.2291082890747,-6.22088499036746));
#3347=CARTESIAN_POINT('Ctrl Pts',(-11.1546995395729,-0.249940827291389,
-6.22004787432886));
#3348=CARTESIAN_POINT('Ctrl Pts',(-11.1642432734415,-0.297768495738485,
-6.21812601017916));
#3349=CARTESIAN_POINT('Ctrl Pts',(-11.1765257430138,-0.345509865059888,
-6.21565068788586));
#3350=CARTESIAN_POINT('Ctrl Pts',(-11.1914688466414,-0.392581270096085,
-6.21267622868436));
#3351=CARTESIAN_POINT('Ctrl Pts',(-11.2067889055284,-0.440840100056904,
-6.20962673567008));
#3352=CARTESIAN_POINT('Ctrl Pts',(-11.2249055260701,-0.488394527974946,
-6.20605265433493));
#3353=CARTESIAN_POINT('Ctrl Pts',(-11.2457345456789,-0.534621239870226,
-6.20206788950022));
#3354=CARTESIAN_POINT('Ctrl Pts',(-11.2578471921851,-0.561503341421173,
-6.19975063939629));
#3355=CARTESIAN_POINT('Ctrl Pts',(-11.2708771019852,-0.587936568342572,
-6.19729554156883));
#3356=CARTESIAN_POINT('Ctrl Pts',(-11.2848077238703,-0.613799570314091,
-6.19473292915621));
#3357=CARTESIAN_POINT('Ctrl Pts',(-11.317012279437,-0.673589182793906,-6.18880872889301));
#3358=CARTESIAN_POINT('Ctrl Pts',(-11.3540305414379,-0.730333687517002,
-6.18230771173298));
#3359=CARTESIAN_POINT('Ctrl Pts',(-11.3943190776739,-0.783294411432698,
-6.17559032328962));
#3360=CARTESIAN_POINT('Ctrl Pts',(-11.4306575667326,-0.831062656853222,
-6.16953153413375));
#3361=CARTESIAN_POINT('Ctrl Pts',(-11.469656504718,-0.87575311065843,-6.16329845093917));
#3362=CARTESIAN_POINT('Ctrl Pts',(-11.5101833773516,-0.916837225683864,
-6.15718080599314));
#3363=CARTESIAN_POINT('Ctrl Pts',(-11.5648237040178,-0.972228854001241,
-6.14893269562692));
#3364=CARTESIAN_POINT('Ctrl Pts',(-11.6274857929233,-1.02318325634266,-6.14057642072509));
#3365=CARTESIAN_POINT('Ctrl Pts',(-11.6956087254554,-1.06850889312374,-6.13267924494715));
#3366=CARTESIAN_POINT('Ctrl Pts',(-11.7680959781152,-1.1167383330964,-6.12427613376803));
#3367=CARTESIAN_POINT('Ctrl Pts',(-11.8467661895401,-1.15859576110227,-6.11639821025487));
#3368=CARTESIAN_POINT('Ctrl Pts',(-11.9285340363439,-1.19266902583605,-6.10974684998498));
#3369=CARTESIAN_POINT('Ctrl Pts',(-11.9925136718482,-1.21932981174788,-6.10454246192402));
#3370=CARTESIAN_POINT('Ctrl Pts',(-12.0583897892245,-1.24122576538538,-6.10009072445943));
#3371=CARTESIAN_POINT('Ctrl Pts',(-12.124684375347,-1.2576802310512,-6.09669635232993));
#3372=CARTESIAN_POINT('Ctrl Pts',(-12.143116210675,-1.26225505411446,-6.09575261752755));
#3373=CARTESIAN_POINT('Ctrl Pts',(-12.161580393752,-1.26640921081734,-6.09489032856723));
#3374=CARTESIAN_POINT('Ctrl Pts',(-12.1800451595059,-1.27012803811809,-6.09411525513559));
#3375=CARTESIAN_POINT('Ctrl Pts',(-12.2370752874949,-1.28161397840879,-6.09172136952683));
#3376=CARTESIAN_POINT('Ctrl Pts',(-12.2941109738721,-1.28894330191908,-6.09016446666203));
#3377=CARTESIAN_POINT('Ctrl Pts',(-12.3512598524599,-1.29234468050352,-6.08944260198454));
#3378=CARTESIAN_POINT('Ctrl Pts',(-12.4111984809399,-1.2959120990134,-6.08868549913693));
#3379=CARTESIAN_POINT('Ctrl Pts',(-12.4712616224261,-1.29515870258049,-6.08884670582411));
#3380=CARTESIAN_POINT('Ctrl Pts',(-12.5315734553096,-1.2903366772538,-6.08986840871161));
#3381=CARTESIAN_POINT('Ctrl Pts',(-12.5395566571344,-1.28969840778749,-6.09000364685586));
#3382=CARTESIAN_POINT('Ctrl Pts',(-12.5475442161835,-1.28898883805471,-6.09015388866053));
#3383=CARTESIAN_POINT('Ctrl Pts',(-12.555536420442,-1.28820853927745,-6.09031893544359));
#3384=CARTESIAN_POINT('Ctrl Pts',(-12.6148621992992,-1.28241641595264,-6.09154407041708));
#3385=CARTESIAN_POINT('Ctrl Pts',(-12.6744439304571,-1.27272832674441,-6.09358899140211));
#3386=CARTESIAN_POINT('Ctrl Pts',(-12.7334612362498,-1.25894040366121,-6.09643625703733));
#3387=CARTESIAN_POINT('Ctrl Pts',(-12.7903656500025,-1.24564610516046,-6.09918158706545));
#3388=CARTESIAN_POINT('Ctrl Pts',(-12.846745329193,-1.22854021111248,-6.10267301592439));
#3389=CARTESIAN_POINT('Ctrl Pts',(-12.9018648908817,-1.20743110787297,-6.10684665730446));
#3390=CARTESIAN_POINT('Ctrl Pts',(-12.9109361860556,-1.20395707976975,-6.10753353382795));
#3391=CARTESIAN_POINT('Ctrl Pts',(-12.9199733510849,-1.20037460654414,-6.10823877499836));
#3392=CARTESIAN_POINT('Ctrl Pts',(-12.9289731080053,-1.19668281244561,-6.1089619594893));
#3393=CARTESIAN_POINT('Ctrl Pts',(-13.0092397676277,-1.16375659200186,-6.11541186740248));
#3394=CARTESIAN_POINT('Ctrl Pts',(-13.0857840883755,-1.12253184392904,-6.12320982866879));
#3395=CARTESIAN_POINT('Ctrl Pts',(-13.1566294645525,-1.07518791339112,-6.13151179783483));
#3396=CARTESIAN_POINT('Ctrl Pts',(-13.2097039744373,-1.03971974249676,-6.13773129963358));
#3397=CARTESIAN_POINT('Ctrl Pts',(-13.2595800061123,-1.00081730251846,-6.14423201250788));
#3398=CARTESIAN_POINT('Ctrl Pts',(-13.305426478321,-0.959409544350473,-6.15069096137168));
#3399=CARTESIAN_POINT('Ctrl Pts',(-13.3207771905434,-0.945545040741119,
-6.15285360247559));
#3400=CARTESIAN_POINT('Ctrl Pts',(-13.3356761479583,-0.93139978266754,-6.15501195034366));
#3401=CARTESIAN_POINT('Ctrl Pts',(-13.3500921536751,-0.917009010794008,
-6.1571552238199));
#3402=CARTESIAN_POINT('Ctrl Pts',(-13.3976333039604,-0.869551076758588,
-6.16422331802285));
#3403=CARTESIAN_POINT('Ctrl Pts',(-13.4425608636519,-0.81703406747505,-6.17148062215402));
#3404=CARTESIAN_POINT('Ctrl Pts',(-13.483600558711,-0.760436921636467,-6.17844654134857));
#3405=CARTESIAN_POINT('Ctrl Pts',(-13.5191371378058,-0.711429029478902,
-6.18447838291243));
#3406=CARTESIAN_POINT('Ctrl Pts',(-13.5517586124413,-0.659362108365003,
-6.1902910582668));
#3407=CARTESIAN_POINT('Ctrl Pts',(-13.5806376553944,-0.604887217003585,
-6.19560952859327));
#3408=CARTESIAN_POINT('Ctrl Pts',(-13.599039804785,-0.570175017901222,-6.19899853582721));
#3409=CARTESIAN_POINT('Ctrl Pts',(-13.6159223677976,-0.534485392014676,
-6.20218766535699));
#3410=CARTESIAN_POINT('Ctrl Pts',(-13.6310712848955,-0.497989969556114,
-6.20511659570644));
#3411=CARTESIAN_POINT('Ctrl Pts',(-13.6491844766246,-0.454353280547129,
-6.2086186464892));
#3412=CARTESIAN_POINT('Ctrl Pts',(-13.6648191782393,-0.409558830596979,
-6.21174609228389));
#3413=CARTESIAN_POINT('Ctrl Pts',(-13.677970884626,-0.364227652922393,-6.21440296351441));
#3414=CARTESIAN_POINT('Ctrl Pts',(-13.6909855338216,-0.319368882682671,
-6.21703214683151));
#3415=CARTESIAN_POINT('Ctrl Pts',(-13.7015686699469,-0.273984691860296,
-6.21920039368607));
#3416=CARTESIAN_POINT('Ctrl Pts',(-13.709715927272,-0.228681285226899,-6.22086576337064));
#3417=CARTESIAN_POINT('Ctrl Pts',(-13.715963806497,-0.193939506265998,-6.2221428837854));
#3418=CARTESIAN_POINT('Ctrl Pts',(-13.7207791744087,-0.159245349452789,
-6.22312532680939));
#3419=CARTESIAN_POINT('Ctrl Pts',(-13.7241600621217,-0.124872935992544,
-6.22381496559358));
#3420=CARTESIAN_POINT('Ctrl Pts',(-13.7279291532591,-0.0865537813983614,
-6.2245837907218));
#3421=CARTESIAN_POINT('Ctrl Pts',(-13.7299154291426,-0.0486342986908554,
-6.22499491309192));
#3422=CARTESIAN_POINT('Ctrl Pts',(-13.7301623651014,-0.0104114932913323,
-6.22505884123977));
#3423=CARTESIAN_POINT('Ctrl Pts',(-13.730182837164,-0.0072426568496272,
-6.22506414116066));
#3424=CARTESIAN_POINT('Ctrl Pts',(-13.7301913545179,-0.00407173538213392,
-6.22506702514711));
#3425=CARTESIAN_POINT('Ctrl Pts',(-13.7301879419361,-0.000898328273157036,
-6.22506748309577));
#3426=CARTESIAN_POINT('Ctrl Pts',(-13.7301342273928,0.0490515694210033,
-6.22507469127552));
#3427=CARTESIAN_POINT('Ctrl Pts',(-13.7271248442808,0.0996193688592282,
-6.22447648964631));
#3428=CARTESIAN_POINT('Ctrl Pts',(-13.7211337179369,0.150256489319034,-6.22325388872313));
#3429=CARTESIAN_POINT('Ctrl Pts',(-13.715142788269,0.200891947469772,-6.22203132793534));
#3430=CARTESIAN_POINT('Ctrl Pts',(-13.7061703111347,0.251596510611804,-6.22018438455461));
#3431=CARTESIAN_POINT('Ctrl Pts',(-13.6941902144386,0.301822616132018,-6.21774630267923));
#3432=CARTESIAN_POINT('Ctrl Pts',(-13.6820411900285,0.35275694474944,-6.21527384214999));
#3433=CARTESIAN_POINT('Ctrl Pts',(-13.6667991289883,0.403199012571096,-6.21219350738699));
#3434=CARTESIAN_POINT('Ctrl Pts',(-13.6484368406936,0.452582026989457,-6.20859368012887));
#3435=CARTESIAN_POINT('Ctrl Pts',(-13.6429068058991,0.467454344840342,-6.20750954673156));
#3436=CARTESIAN_POINT('Ctrl Pts',(-13.6370937698569,0.482230648591652,-6.20637865560157));
#3437=CARTESIAN_POINT('Ctrl Pts',(-13.6309969898517,0.496895573243171,-6.20520432905971));
#3438=CARTESIAN_POINT('Ctrl Pts',(-13.6095308024466,0.548529389877824,-6.2010696360577));
#3439=CARTESIAN_POINT('Ctrl Pts',(-13.5845471044433,0.598788311474538,-6.19639176855541));
#3440=CARTESIAN_POINT('Ctrl Pts',(-13.5566725551178,0.647027314399991,-6.19135054980013));
#3441=CARTESIAN_POINT('Ctrl Pts',(-13.5257682528023,0.700509532619786,-6.1857613886398));
#3442=CARTESIAN_POINT('Ctrl Pts',(-13.4913105190966,0.7515085229059,-6.17972570509742));
#3443=CARTESIAN_POINT('Ctrl Pts',(-13.4541533675084,0.799161663499016,-6.17355704692874));
#3444=CARTESIAN_POINT('Ctrl Pts',(-13.421364771179,0.841212238528311,-6.16811363606592));
#3445=CARTESIAN_POINT('Ctrl Pts',(-13.3864741834141,0.880657802541923,-6.1625685925932));
#3446=CARTESIAN_POINT('Ctrl Pts',(-13.3500684256529,0.916916483466317,-6.15716900356307));
#3447=CARTESIAN_POINT('Ctrl Pts',(-13.3072843024532,0.959527761657628,-6.1508233951621));
#3448=CARTESIAN_POINT('Ctrl Pts',(-13.2602024392506,1.000011743866,-6.14433750063204));
#3449=CARTESIAN_POINT('Ctrl Pts',(-13.2096808645379,1.03743921852613,-6.13801155456341));
#3450=CARTESIAN_POINT('Ctrl Pts',(-13.1477978650733,1.08328348223975,-6.13026301308574));
#3451=CARTESIAN_POINT('Ctrl Pts',(-13.0807541375615,1.12454175109865,-6.12275592889658));
#3452=CARTESIAN_POINT('Ctrl Pts',(-13.0101265129726,1.15953221587873,-6.11612222052743));
#3453=CARTESIAN_POINT('Ctrl Pts',(-12.9835946088692,1.17267669952065,-6.11363020815516));
#3454=CARTESIAN_POINT('Ctrl Pts',(-12.9565569462931,1.18493690018302,-6.11126196523134));
#3455=CARTESIAN_POINT('Ctrl Pts',(-12.9290971176065,1.19622424046656,-6.10905177115158));
#3456=CARTESIAN_POINT('Ctrl Pts',(-12.8721127877878,1.21964760296576,-6.10446520108074));
#3457=CARTESIAN_POINT('Ctrl Pts',(-12.8133104381631,1.23887976609541,-6.10056386132526));
#3458=CARTESIAN_POINT('Ctrl Pts',(-12.75381277262,1.25394388410792,-6.09746592541511));
#3459=CARTESIAN_POINT('Ctrl Pts',(-12.694302849074,1.2690111057044,-6.09436735125291));
#3460=CARTESIAN_POINT('Ctrl Pts',(-12.6340973230754,1.27990869110762,-6.09207248827396));
#3461=CARTESIAN_POINT('Ctrl Pts',(-12.5743195925698,1.28665074919624,-6.09064822705127));
#3462=CARTESIAN_POINT('Ctrl Pts',(-12.5258076391736,1.29212219157157,-6.08949238367156));
#3463=CARTESIAN_POINT('Ctrl Pts',(-12.4775774299124,1.29485665783831,-6.08890895085005));
#3464=CARTESIAN_POINT('Ctrl Pts',(-12.4302293937643,1.29485665783831,-6.08890895085005));
#3465=CARTESIAN_POINT('Origin',(-12.4302293937643,0.,0.));
#3466=CARTESIAN_POINT('',(-13.4302293937643,9.49101269339199E-16,4.5));
#3467=CARTESIAN_POINT('Origin',(-12.4302293937643,8.26636589424463E-16,
4.5));
#3468=CARTESIAN_POINT('',(-13.4302293937643,-1.22464679914735E-16,2.24963967399279E-32));
#3469=CARTESIAN_POINT('Ctrl Pts',(-12.4302293937643,6.08898133099087,1.29494387859312));
#3470=CARTESIAN_POINT('Ctrl Pts',(-12.5942619533871,6.08898130876529,1.29494384540356));
#3471=CARTESIAN_POINT('Ctrl Pts',(-12.9435374583722,6.10366925625812,1.22945303091367));
#3472=CARTESIAN_POINT('Ctrl Pts',(-13.2353404857064,6.14038646272546,1.03141337526286));
#3473=CARTESIAN_POINT('Ctrl Pts',(-13.4654395118979,6.17439967538392,0.802430842761209));
#3474=CARTESIAN_POINT('Ctrl Pts',(-13.6642427239162,6.21076528208221,0.511664182013643));
#3475=CARTESIAN_POINT('Ctrl Pts',(-13.7306321021329,6.22545881283488,0.163545778636827));
#3476=CARTESIAN_POINT('Ctrl Pts',(-13.7305989411604,6.22543847090119,-0.163641090648478));
#3477=CARTESIAN_POINT('Ctrl Pts',(-13.6642156833053,6.21072435088059,-0.511783667678438));
#3478=CARTESIAN_POINT('Ctrl Pts',(-13.4653424297833,6.17435111576691,-0.802515858885917));
#3479=CARTESIAN_POINT('Ctrl Pts',(-13.2353573393715,6.1402285928138,-1.03175436379926));
#3480=CARTESIAN_POINT('Ctrl Pts',(-13.0895788709221,6.12205139295494,-1.13084360876944));
#3481=CARTESIAN_POINT('Ctrl Pts',(-12.7689529244921,6.09609767279734,-1.26292405472951));
#3482=CARTESIAN_POINT('Ctrl Pts',(-12.5945528226149,6.08914675284976,-1.29475090526595));
#3483=CARTESIAN_POINT('Ctrl Pts',(-12.1420480242785,6.08829833850425,-1.29750804265229));
#3484=CARTESIAN_POINT('Ctrl Pts',(-11.7821275442938,6.1174178096963,-1.17136422515573));
#3485=CARTESIAN_POINT('Ctrl Pts',(-11.5389300175645,6.15310688833719,-0.945622018154235));
#3486=CARTESIAN_POINT('Ctrl Pts',(-11.3949322424527,6.17435262252434,-0.802915209412389));
#3487=CARTESIAN_POINT('Ctrl Pts',(-11.2460566890049,6.20152475294844,-0.584204969074392));
#3488=CARTESIAN_POINT('Ctrl Pts',(-11.1584525181573,6.21935644205315,-0.293078203033809));
#3489=CARTESIAN_POINT('Ctrl Pts',(-11.1341427705081,6.22436148348913,-0.123532917714704));
#3490=CARTESIAN_POINT('Ctrl Pts',(-11.1219312944025,6.22705283541575,0.121373316802368));
#3491=CARTESIAN_POINT('Ctrl Pts',(-11.195852637914,6.21080281923344,0.510717187316461));
#3492=CARTESIAN_POINT('Ctrl Pts',(-11.3953251934327,6.17426182590549,0.802628398668338));
#3493=CARTESIAN_POINT('Ctrl Pts',(-11.6251545032248,6.14020379361964,1.03156839761272));
#3494=CARTESIAN_POINT('Ctrl Pts',(-11.7709691894469,6.12201232016596,1.13070854621628));
#3495=CARTESIAN_POINT('Ctrl Pts',(-12.0914612527931,6.09613472840634,1.26250865035172));
#3496=CARTESIAN_POINT('Ctrl Pts',(-12.2661968588882,6.08898130665445,1.29494390504147));
#3497=CARTESIAN_POINT('Ctrl Pts',(-12.4302293937643,6.08898133099087,1.29494387859312));
#3498=CARTESIAN_POINT('Ctrl Pts',(-12.4302293937643,6.00722696133003,1.19642683026457));
#3499=CARTESIAN_POINT('Ctrl Pts',(-12.5835311917541,6.00725206547108,1.19646431839136));
#3500=CARTESIAN_POINT('Ctrl Pts',(-12.909964007985,6.02008795273409,1.13389253469307));
#3501=CARTESIAN_POINT('Ctrl Pts',(-13.1794216562216,6.05199550620319,0.947617208560084));
#3502=CARTESIAN_POINT('Ctrl Pts',(-13.3904648409007,6.08141552880984,0.734503844042364));
#3503=CARTESIAN_POINT('Ctrl Pts',(-13.570887885006,6.11264821229161,0.465895827821163));
#3504=CARTESIAN_POINT('Ctrl Pts',(-13.63034543552,6.12520612798745,0.148902652084511));
#3505=CARTESIAN_POINT('Ctrl Pts',(-13.6303230222317,6.12518235248142,-0.148993075746921));
#3506=CARTESIAN_POINT('Ctrl Pts',(-13.570842515833,6.11261315450347,-0.466033199953071));
#3507=CARTESIAN_POINT('Ctrl Pts',(-13.3903856984601,6.08136116262512,-0.734565587427399));
#3508=CARTESIAN_POINT('Ctrl Pts',(-13.179410253184,6.05184812885104,-0.948000402118588));
#3509=CARTESIAN_POINT('Ctrl Pts',(-13.044873465078,6.03604579828012,-1.04111526370645));
#3510=CARTESIAN_POINT('Ctrl Pts',(-12.7467548427922,6.01347833294355,-1.16594234995302));
#3511=CARTESIAN_POINT('Ctrl Pts',(-12.5838837655095,6.00734418127635,-1.19625532919237));
#3512=CARTESIAN_POINT('Ctrl Pts',(-12.1607096950123,6.00667035326614,-1.19893255050596));
#3513=CARTESIAN_POINT('Ctrl Pts',(-11.8251276746147,6.03213208496433,-1.07836492136828));
#3514=CARTESIAN_POINT('Ctrl Pts',(-11.6020268212092,6.06296598113213,-0.867855162821189));
#3515=CARTESIAN_POINT('Ctrl Pts',(-11.4699415156986,6.08136857971696,-0.734854564014157));
#3516=CARTESIAN_POINT('Ctrl Pts',(-11.3347377808286,6.10471391255857,-0.533003961090166));
#3517=CARTESIAN_POINT('Ctrl Pts',(-11.2558516212822,6.11997308110787,-0.266984478934218));
#3518=CARTESIAN_POINT('Ctrl Pts',(-11.2339578831136,6.1242543025212,-0.112499763704596));
#3519=CARTESIAN_POINT('Ctrl Pts',(-11.2230782222799,6.12653186075723,0.110502918514062));
#3520=CARTESIAN_POINT('Ctrl Pts',(-11.2892260889657,6.11268306432087,0.465058908284595));
#3521=CARTESIAN_POINT('Ctrl Pts',(-11.4702873307785,6.08127779974347,0.734631343754487));
#3522=CARTESIAN_POINT('Ctrl Pts',(-11.681094900266,6.05181289859711,0.947846902939449));
#3523=CARTESIAN_POINT('Ctrl Pts',(-11.8156864487299,6.03603021308043,1.04095287446958));
#3524=CARTESIAN_POINT('Ctrl Pts',(-12.1136410603724,6.01347722311489,1.16555887365695));
#3525=CARTESIAN_POINT('Ctrl Pts',(-12.2768996439547,6.0072544496917,1.19639695643086));
#3526=CARTESIAN_POINT('Ctrl Pts',(-12.4302293937643,6.00722696133003,1.19642683026457));
#3527=CARTESIAN_POINT('Ctrl Pts',(-12.4302293937643,5.9254725916692,1.09790978193603));
#3528=CARTESIAN_POINT('Ctrl Pts',(-12.5728345397284,5.92544735481571,1.09787209562915));
#3529=CARTESIAN_POINT('Ctrl Pts',(-12.8763450487991,5.93647960612607,1.03842675040526));
#3530=CARTESIAN_POINT('Ctrl Pts',(-13.1235630570658,5.96359104894073,0.863676007684786));
#3531=CARTESIAN_POINT('Ctrl Pts',(-13.3154843928422,5.98836813882517,0.666454964337181));
#3532=CARTESIAN_POINT('Ctrl Pts',(-13.4776843866789,6.0145609350393,0.420230715694402));
#3533=CARTESIAN_POINT('Ctrl Pts',(-13.5299505040167,6.0248593589734,0.134217204930517));
#3534=CARTESIAN_POINT('Ctrl Pts',(-13.5299007211169,6.02484699389389,-0.134415017109032));
#3535=CARTESIAN_POINT('Ctrl Pts',(-13.4776660945839,6.01452487292353,-0.420420663484723));
#3536=CARTESIAN_POINT('Ctrl Pts',(-13.3153544274694,5.98833547677297,-0.666673705537073));
#3537=CARTESIAN_POINT('Ctrl Pts',(-13.1235774765046,5.96346920539124,-0.864075760813053));
#3538=CARTESIAN_POINT('Ctrl Pts',(-13.0001273339958,5.9500823476246,-0.951353330164833));
#3539=CARTESIAN_POINT('Ctrl Pts',(-12.7246790600745,5.93077700575973,-1.06883672236603));
#3540=CARTESIAN_POINT('Ctrl Pts',(-12.5731730637106,5.92562762457043,-1.09763635624804));
#3541=CARTESIAN_POINT('Ctrl Pts',(-12.1795045349912,5.92492523315675,-1.10023761151678));
#3542=CARTESIAN_POINT('Ctrl Pts',(-11.8682715322971,5.94673197605431,-0.98542923697083));
#3543=CARTESIAN_POINT('Ctrl Pts',(-11.6651441685123,5.97286503936011,-0.789835019063647));
#3544=CARTESIAN_POINT('Ctrl Pts',(-11.5449751521618,5.98831895514578,-0.667076440523771));
#3545=CARTESIAN_POINT('Ctrl Pts',(-11.4234880389121,6.00790204058972,-0.48164167101503));
#3546=CARTESIAN_POINT('Ctrl Pts',(-11.3532980958741,6.02055638021736,-0.240902614043722));
#3547=CARTESIAN_POINT('Ctrl Pts',(-11.3338748805631,6.0241045391149,-0.101410210808414));
#3548=CARTESIAN_POINT('Ctrl Pts',(-11.324192538491,6.02601447481949,0.0996219915262307));
#3549=CARTESIAN_POINT('Ctrl Pts',(-11.3825655879323,6.01457216711308,0.419448146088014));
#3550=CARTESIAN_POINT('Ctrl Pts',(-11.5452549217081,5.98827602700875,0.666788336702704));
#3551=CARTESIAN_POINT('Ctrl Pts',(-11.7369439829688,5.96346321923707,0.863887776934397));
#3552=CARTESIAN_POINT('Ctrl Pts',(-11.8604202279154,5.95003321189189,0.951280997109748));
#3553=CARTESIAN_POINT('Ctrl Pts',(-12.1357679453513,5.93083589668504,1.06847119991178));
#3554=CARTESIAN_POINT('Ctrl Pts',(-12.2876523473866,5.92544495799094,1.09793981369705));
#3555=CARTESIAN_POINT('Ctrl Pts',(-12.4302293937643,5.9254725916692,1.09790978193603));
#3556=CARTESIAN_POINT('Ctrl Pts',(-12.4302293937643,5.84371822200836,0.999392733607483));
#3557=CARTESIAN_POINT('Ctrl Pts',(-12.5621036578468,5.84371837757123,0.99939296591021));
#3558=CARTESIAN_POINT('Ctrl Pts',(-12.8427717588467,5.8528983979387,0.942865920290856));
#3559=CARTESIAN_POINT('Ctrl Pts',(-13.0676440152473,5.87520014001345,0.779880352279897));
#3560=CARTESIAN_POINT('Ctrl Pts',(-13.2405097422111,5.89538421520699,0.598528395292872));
#3561=CARTESIAN_POINT('Ctrl Pts',(-13.3843290142384,5.91644376021923,0.374461997536319));
#3562=CARTESIAN_POINT('Ctrl Pts',(-13.4296642190767,5.92460700580665,0.119574227573619));
#3563=CARTESIAN_POINT('Ctrl Pts',(-13.4296253182383,5.92459115482435,-0.119766755586355));
#3564=CARTESIAN_POINT('Ctrl Pts',(-13.3842922335101,5.91641359576347,-0.374669709501813));
#3565=CARTESIAN_POINT('Ctrl Pts',(-13.2403979589254,5.8953456496019,-0.59872322823422));
#3566=CARTESIAN_POINT('Ctrl Pts',(-13.0676299873348,5.87508873599765,-0.780322400839761));
#3567=CARTESIAN_POINT('Ctrl Pts',(-12.9554220717229,5.86407660437688,-0.861625103513371));
#3568=CARTESIAN_POINT('Ctrl Pts',(-12.7024805472264,5.84815795494093,-0.971855454462235));
#3569=CARTESIAN_POINT('Ctrl Pts',(-12.5625041534178,5.84382474976352,-0.999141215193046));
#3570=CARTESIAN_POINT('Ctrl Pts',(-12.1981657362553,5.8432976608614,-1.00166254046375));
#3571=CARTESIAN_POINT('Ctrl Pts',(-11.9112711559271,5.86144665456792,-0.892429708902027));
#3572=CARTESIAN_POINT('Ctrl Pts',(-11.7282408997332,5.88272399126246,-0.712069056663859));
#3573=CARTESIAN_POINT('Ctrl Pts',(-11.6199843395186,5.89533514353784,-0.599014799133686));
#3574=CARTESIAN_POINT('Ctrl Pts',(-11.5121688868997,5.91109120383654,-0.430441231608476));
#3575=CARTESIAN_POINT('Ctrl Pts',(-11.4506970319975,5.92117313680743,-0.214808848136133));
#3576=CARTESIAN_POINT('Ctrl Pts',(-11.4336896339877,5.92399750826545,-0.0903772556247663));
#3577=CARTESIAN_POINT('Ctrl Pts',(-11.4253395813362,5.92549348750944,0.0887516303553966));
#3578=CARTESIAN_POINT('Ctrl Pts',(-11.4759391586775,5.91645238097389,0.373789699542128));
#3579=CARTESIAN_POINT('Ctrl Pts',(-11.6202170398282,5.8952920634098,0.598790738714452));
#3580=CARTESIAN_POINT('Ctrl Pts',(-11.792884701926,5.87507217891444,0.780167119997466));
#3581=CARTESIAN_POINT('Ctrl Pts',(-11.9051374289599,5.86405115731345,0.861525029957537));
#3582=CARTESIAN_POINT('Ctrl Pts',(-12.1579479395019,5.84817833435726,0.971521909353962));
#3583=CARTESIAN_POINT('Ctrl Pts',(-12.2983549564728,5.84371839234553,0.999392548488257));
#3584=CARTESIAN_POINT('Ctrl Pts',(-12.4302293937643,5.84371822200836,0.999392733607483));
#3585=CARTESIAN_POINT('',(-12.4302293937643,5.84422216200635,1.));
#3586=CARTESIAN_POINT('',(-12.4302293937643,6.08890895085005,1.29485665783831));
#3587=CARTESIAN_POINT('',(-13.4302293891297,5.92521705509939,-9.62763526687191E-5));
#3588=CARTESIAN_POINT('Ctrl Pts',(-12.4302293937643,5.84422216200635,0.999999999999999));
#3589=CARTESIAN_POINT('Ctrl Pts',(-12.4592320214116,5.84422216200635,0.999999999999999));
#3590=CARTESIAN_POINT('Ctrl Pts',(-12.4886478834784,5.8444442230921,0.998734139041022));
#3591=CARTESIAN_POINT('Ctrl Pts',(-12.5182411890796,5.84487442357384,0.996119432540782));
#3592=CARTESIAN_POINT('Ctrl Pts',(-12.5476087369448,5.84530134219555,0.993524672788903));
#3593=CARTESIAN_POINT('Ctrl Pts',(-12.5771503766343,5.84593323667031,0.989601419867018));
#3594=CARTESIAN_POINT('Ctrl Pts',(-12.6066265082011,5.84675650149613,0.984319083437057));
#3595=CARTESIAN_POINT('Ctrl Pts',(-12.6360181252477,5.84757740584151,0.979051892621711));
#3596=CARTESIAN_POINT('Ctrl Pts',(-12.6653439314479,5.84858858470984,0.972433382071454));
#3597=CARTESIAN_POINT('Ctrl Pts',(-12.6943672114053,5.84977654929374,0.96448494715668));
#3598=CARTESIAN_POINT('Ctrl Pts',(-12.7233731679207,5.85096380480425,0.956541256511066));
#3599=CARTESIAN_POINT('Ctrl Pts',(-12.7520762879357,5.85232763505328,0.94726936028975));
#3600=CARTESIAN_POINT('Ctrl Pts',(-12.7802512593826,5.85385457537269,0.936741529766411));
#3601=CARTESIAN_POINT('Ctrl Pts',(-12.7967306907133,5.85474767683288,0.930583842597197));
#3602=CARTESIAN_POINT('Ctrl Pts',(-12.8130297003045,5.85569657881332,0.923997448220513));
#3603=CARTESIAN_POINT('Ctrl Pts',(-12.8291063084377,5.8566985871014,0.917004474874906));
#3604=CARTESIAN_POINT('Ctrl Pts',(-12.8575304396385,5.85847018063709,0.904640598725699));
#3605=CARTESIAN_POINT('Ctrl Pts',(-12.8853056660692,5.86040778318034,0.890982659342418));
#3606=CARTESIAN_POINT('Ctrl Pts',(-12.9122329134691,5.86246204056025,0.876169279872447));
#3607=CARTESIAN_POINT('Ctrl Pts',(-12.939327595744,5.86452907140796,0.861263790120844));
#3608=CARTESIAN_POINT('Ctrl Pts',(-12.9655631808851,5.86671421233306,0.845188887893915));
#3609=CARTESIAN_POINT('Ctrl Pts',(-12.9907703544572,5.86896718276849,0.828126700080028));
#3610=CARTESIAN_POINT('Ctrl Pts',(-13.0161011819465,5.87123120516175,0.810980813617723));
#3611=CARTESIAN_POINT('Ctrl Pts',(-13.040393080685,5.87356372417359,0.792838498440963));
#3612=CARTESIAN_POINT('Ctrl Pts',(-13.0635150989357,5.87591371564642,0.773918093615534));
#3613=CARTESIAN_POINT('Ctrl Pts',(-13.0869035542154,5.87829078627554,0.754779667318463));
#3614=CARTESIAN_POINT('Ctrl Pts',(-13.1090947171264,5.88068573435905,0.734845746588785));
#3615=CARTESIAN_POINT('Ctrl Pts',(-13.1300001719029,5.88304575146868,0.714367453110294));
#3616=CARTESIAN_POINT('Ctrl Pts',(-13.1383433794932,5.88398761630122,0.706194722336734));
#3617=CARTESIAN_POINT('Ctrl Pts',(-13.1464823508734,5.88492391751257,0.6979355119476));
#3618=CARTESIAN_POINT('Ctrl Pts',(-13.1544136476108,5.88585129831765,0.689606530190082));
#3619=CARTESIAN_POINT('Ctrl Pts',(-13.1760213569284,5.88837781769102,0.666915383623946));
#3620=CARTESIAN_POINT('Ctrl Pts',(-13.1967993780494,5.89093180677019,0.642953073760821));
#3621=CARTESIAN_POINT('Ctrl Pts',(-13.2165148917462,5.893455949781,0.617863347078739));
#3622=CARTESIAN_POINT('Ctrl Pts',(-13.235525524171,5.89588984806556,0.59367064386409));
#3623=CARTESIAN_POINT('Ctrl Pts',(-13.2535478793342,5.89829599628131,0.568430356987537));
#3624=CARTESIAN_POINT('Ctrl Pts',(-13.270406707377,5.90062300904914,0.54231179379622));
#3625=CARTESIAN_POINT('Ctrl Pts',(-13.2872366276282,5.90294603169379,0.516238016042039));
#3626=CARTESIAN_POINT('Ctrl Pts',(-13.302906563573,5.90519019004457,0.489289499082407));
#3627=CARTESIAN_POINT('Ctrl Pts',(-13.3172825639117,5.9073043626005,0.461667275569134));
#3628=CARTESIAN_POINT('Ctrl Pts',(-13.331660445953,5.90941881188457,0.434041436529585));
#3629=CARTESIAN_POINT('Ctrl Pts',(-13.3447437328419,5.9114032413434,0.405742328697114));
#3630=CARTESIAN_POINT('Ctrl Pts',(-13.3564446413391,5.91320650939921,0.376995112912612));
#3631=CARTESIAN_POINT('Ctrl Pts',(-13.3577869138172,5.91341337171956,0.373697369273322));
#3632=CARTESIAN_POINT('Ctrl Pts',(-13.3591110475612,5.91361785003098,0.370393748670391));
#3633=CARTESIAN_POINT('Ctrl Pts',(-13.3604169514719,5.91381986712987,0.367084605351364));
#3634=CARTESIAN_POINT('Ctrl Pts',(-13.3723151401828,5.9156604601059,0.336934751784082));
#3635=CARTESIAN_POINT('Ctrl Pts',(-13.3827086173401,5.91729674366869,0.306293119193863));
#3636=CARTESIAN_POINT('Ctrl Pts',(-13.3915566759856,5.91871491003209,0.2754085264783));
#3637=CARTESIAN_POINT('Ctrl Pts',(-13.4004276260277,5.9201367454273,0.244444030194534));
#3638=CARTESIAN_POINT('Ctrl Pts',(-13.4077451239213,5.92133933355236,0.213236017734468));
#3639=CARTESIAN_POINT('Ctrl Pts',(-13.413520678218,5.92230875917455,0.182039143915082));
#3640=CARTESIAN_POINT('Ctrl Pts',(-13.4193449731899,5.92328636590921,0.15057899550552));
#3641=CARTESIAN_POINT('Ctrl Pts',(-13.4236012816078,5.92402685815631,0.119130873576328));
#3642=CARTESIAN_POINT('Ctrl Pts',(-13.4263543498779,5.92451596540413,0.0879492570048032));
#3643=CARTESIAN_POINT('Ctrl Pts',(-13.4289729319664,5.9249811799767,0.0582908487725101));
#3644=CARTESIAN_POINT('Ctrl Pts',(-13.4302321782768,5.9252189697697,0.028873943407611));
#3645=CARTESIAN_POINT('Ctrl Pts',(-13.4302293891297,5.92521705509939,-9.62763526685966E-5));
#3646=CARTESIAN_POINT('Ctrl Pts',(-13.4302293891297,5.92521705509939,-9.62763526688415E-5));
#3647=CARTESIAN_POINT('Ctrl Pts',(-13.4302264582134,5.92521504310856,-0.0305390195007855));
#3648=CARTESIAN_POINT('Ctrl Pts',(-13.4288294590287,5.92494889813534,-0.0614755629460699));
#3649=CARTESIAN_POINT('Ctrl Pts',(-13.4259265463018,5.9244327519576,-0.0926670406820359));
#3650=CARTESIAN_POINT('Ctrl Pts',(-13.4230403352885,5.92391957539228,-0.123679060342671));
#3651=CARTESIAN_POINT('Ctrl Pts',(-13.4186652254003,5.92315926607723,-0.154942467869905));
#3652=CARTESIAN_POINT('Ctrl Pts',(-13.4127399837538,5.92216571327227,-0.186206714590468));
#3653=CARTESIAN_POINT('Ctrl Pts',(-13.4068458877949,5.92117738301978,-0.21730662261883));
#3654=CARTESIAN_POINT('Ctrl Pts',(-13.3994178054916,5.91995825489446,-0.248406687039036));
#3655=CARTESIAN_POINT('Ctrl Pts',(-13.3904465693376,5.91852200028117,-0.279254320886848));
#3656=CARTESIAN_POINT('Ctrl Pts',(-13.3818241197141,5.9171415848248,-0.308902650759479));
#3657=CARTESIAN_POINT('Ctrl Pts',(-13.371776487637,5.915560597712,-0.338317213207077));
#3658=CARTESIAN_POINT('Ctrl Pts',(-13.3603408425699,5.91379117695691,-0.367277405785775));
#3659=CARTESIAN_POINT('Ctrl Pts',(-13.3485095199021,5.91196053358123,-0.397239631870212));
#3660=CARTESIAN_POINT('Ctrl Pts',(-13.3351782714556,5.90992819122401,-0.426748421701383));
#3661=CARTESIAN_POINT('Ctrl Pts',(-13.3204401056177,5.90775093729684,-0.455548996817583));
#3662=CARTESIAN_POINT('Ctrl Pts',(-13.3062511503052,5.90565481766999,-0.483276332619849));
#3663=CARTESIAN_POINT('Ctrl Pts',(-13.2907588121517,5.9034243853599,-0.510346745426924));
#3664=CARTESIAN_POINT('Ctrl Pts',(-13.2740937370534,5.90111031294684,-0.536556586135456));
#3665=CARTESIAN_POINT('Ctrl Pts',(-13.2574071915474,5.8987932592044,-0.562800194226458));
#3666=CARTESIAN_POINT('Ctrl Pts',(-13.2395453245768,5.89639234970513,-0.588180474034698));
#3667=CARTESIAN_POINT('Ctrl Pts',(-13.2206804853333,5.89395845313342,-0.612525160166824));
#3668=CARTESIAN_POINT('Ctrl Pts',(-13.2017317678401,5.89151373478996,-0.636978089450959));
#3669=CARTESIAN_POINT('Ctrl Pts',(-13.1817716774107,5.88903573538278,-0.660385759745594));
#3670=CARTESIAN_POINT('Ctrl Pts',(-13.1610090523917,5.88657600514603,-0.682613426864979));
#3671=CARTESIAN_POINT('Ctrl Pts',(-13.1587569437218,5.88630919977885,-0.685024447715524));
#3672=CARTESIAN_POINT('Ctrl Pts',(-13.156495420895,5.88604260935945,-0.687421627037074));
#3673=CARTESIAN_POINT('Ctrl Pts',(-13.1542247700728,5.88577629967664,-0.689804823905987));
#3674=CARTESIAN_POINT('Ctrl Pts',(-13.1339907182747,5.88340318098149,-0.711041787519624));
#3675=CARTESIAN_POINT('Ctrl Pts',(-13.1124165710007,5.88098167042095,-0.731808711400977));
#3676=CARTESIAN_POINT('Ctrl Pts',(-13.089570727107,5.87856224500728,-0.751843737851061));
#3677=CARTESIAN_POINT('Ctrl Pts',(-13.0670118937186,5.8761732146411,-0.771627065870116));
#3678=CARTESIAN_POINT('Ctrl Pts',(-13.043213336531,5.87378621735982,-0.790696138338821));
#3679=CARTESIAN_POINT('Ctrl Pts',(-13.018287850596,5.87144985155954,-0.808818429159916));
#3680=CARTESIAN_POINT('Ctrl Pts',(-12.9935019925622,5.86912657364263,-0.826839202303933));
#3681=CARTESIAN_POINT('Ctrl Pts',(-12.9676021277528,5.86685336153941,-0.843923179825897));
#3682=CARTESIAN_POINT('Ctrl Pts',(-12.9407418268909,5.86467800149521,-0.859870371406732));
#3683=CARTESIAN_POINT('Ctrl Pts',(-12.9140104238785,5.86251308062044,-0.875741035226008));
#3684=CARTESIAN_POINT('Ctrl Pts',(-12.8863282483644,5.86044507490852,-0.890485297091702));
#3685=CARTESIAN_POINT('Ctrl Pts',(-12.8578830598608,5.85852108594758,-0.903942665147648));
#3686=CARTESIAN_POINT('Ctrl Pts',(-12.8483500352163,5.85787628676904,-0.908452722140648));
#3687=CARTESIAN_POINT('Ctrl Pts',(-12.8387315828453,5.85724766305677,-0.91281857737988));
#3688=CARTESIAN_POINT('Ctrl Pts',(-12.8290355364334,5.85663698778019,-0.917035255903188));
#3689=CARTESIAN_POINT('Ctrl Pts',(-12.8006813737891,5.85485118917947,-0.929366095050314));
#3690=CARTESIAN_POINT('Ctrl Pts',(-12.7716621236898,5.85324772267947,-0.940417687690155));
#3691=CARTESIAN_POINT('Ctrl Pts',(-12.7421979764678,5.85183237825636,-0.950092418349892));
#3692=CARTESIAN_POINT('Ctrl Pts',(-12.7126954949783,5.85041519240232,-0.959779736297889));
#3693=CARTESIAN_POINT('Ctrl Pts',(-12.6827476165911,5.84918661845529,-0.968086386359692));
#3694=CARTESIAN_POINT('Ctrl Pts',(-12.6525913531979,5.84815246901999,-0.97496418344309));
#3695=CARTESIAN_POINT('Ctrl Pts',(-12.6223845035406,5.84711658482876,-0.981853517833188));
#3696=CARTESIAN_POINT('Ctrl Pts',(-12.5919692612567,5.84627577797941,-0.987309141862486));
#3697=CARTESIAN_POINT('Ctrl Pts',(-12.5615896425454,5.84563589037716,-0.991334698797625));
#3698=CARTESIAN_POINT('Ctrl Pts',(-12.5310315251629,5.84499224304745,-0.995383908319399));
#3699=CARTESIAN_POINT('Ctrl Pts',(-12.5005101422583,5.84455188294582,-0.997986271070962));
#3700=CARTESIAN_POINT('Ctrl Pts',(-12.4702692367735,5.84432075555793,-0.999198083951227));
#3701=CARTESIAN_POINT('Ctrl Pts',(-12.4567895079721,5.84421773170804,-0.999738243338723));
#3702=CARTESIAN_POINT('Ctrl Pts',(-12.4433653826999,5.84415627999187,-1.00000280430924));
#3703=CARTESIAN_POINT('Ctrl Pts',(-12.4300176179556,5.84413692696769,-0.999999977575504));
#3704=CARTESIAN_POINT('Ctrl Pts',(-12.3997273096931,5.84409300882263,-0.999993562820831));
#3705=CARTESIAN_POINT('Ctrl Pts',(-12.3690627220166,5.84432630738648,-0.998606698701212));
#3706=CARTESIAN_POINT('Ctrl Pts',(-12.3382632274432,5.84480595565223,-0.995762132365058));
#3707=CARTESIAN_POINT('Ctrl Pts',(-12.3075934980838,5.8452835830517,-0.992929550828145));
#3708=CARTESIAN_POINT('Ctrl Pts',(-12.2767906587517,5.84600548867243,-0.988651368556739));
#3709=CARTESIAN_POINT('Ctrl Pts',(-12.2460999634423,5.84694119401489,-0.9829020057408));
#3710=CARTESIAN_POINT('Ctrl Pts',(-12.2154843590106,5.8478746099685,-0.97716670988216));
#3711=CARTESIAN_POINT('Ctrl Pts',(-12.1849810389625,5.8490207807168,-0.969967418608316));
#3712=CARTESIAN_POINT('Ctrl Pts',(-12.1548321948058,5.85034945092846,-0.961330527345209));
#3713=CARTESIAN_POINT('Ctrl Pts',(-12.1247087433682,5.85167700207402,-0.952700910462241));
#3714=CARTESIAN_POINT('Ctrl Pts',(-12.094939848471,5.85318674539381,-0.942636261039028));
#3715=CARTESIAN_POINT('Ctrl Pts',(-12.0657555508963,5.85484850193932,-0.931213626331269));
#3716=CARTESIAN_POINT('Ctrl Pts',(-12.0364962427691,5.85651452959249,-0.91976163274865));
#3717=CARTESIAN_POINT('Ctrl Pts',(-12.0078251817651,5.85833335289554,-0.906944943031127));
#3718=CARTESIAN_POINT('Ctrl Pts',(-11.9799526239205,5.86027455960027,-0.892889035960829));
#3719=CARTESIAN_POINT('Ctrl Pts',(-11.9520165849043,5.86222018750224,-0.878801115845509));
#3720=CARTESIAN_POINT('Ctrl Pts',(-11.9248832439706,5.86428875690958,-0.863468752525495));
#3721=CARTESIAN_POINT('Ctrl Pts',(-11.8987336381442,5.86644964730411,-0.847060955160747));
#3722=CARTESIAN_POINT('Ctrl Pts',(-11.8723903943151,5.8686265391062,-0.83053165794883));
#3723=CARTESIAN_POINT('Ctrl Pts',(-11.8470459767866,5.87089712423285,-0.812911460103129));
#3724=CARTESIAN_POINT('Ctrl Pts',(-11.8228465976897,5.87323009688088,-0.794409301954961));
#3725=CARTESIAN_POINT('Ctrl Pts',(-11.8066067163169,5.874795723788,-0.781992749767297));
#3726=CARTESIAN_POINT('Ctrl Pts',(-11.7908816808213,5.87638944737418,-0.769179747345653));
#3727=CARTESIAN_POINT('Ctrl Pts',(-11.7757046159195,5.87800180612318,-0.756040551284902));
#3728=CARTESIAN_POINT('Ctrl Pts',(-11.7563448014304,5.88005852568473,-0.739280235643044));
#3729=CARTESIAN_POINT('Ctrl Pts',(-11.7378440338808,5.88214556739628,-0.72195704287926));
#3730=CARTESIAN_POINT('Ctrl Pts',(-11.720315065076,5.88417207266275,-0.704288041871364));
#3731=CARTESIAN_POINT('Ctrl Pts',(-11.7155619706134,5.8847215728112,-0.699496976761671));
#3732=CARTESIAN_POINT('Ctrl Pts',(-11.7108800779854,5.88526662196504,-0.694680646620972));
#3733=CARTESIAN_POINT('Ctrl Pts',(-11.7062710700307,5.88580540867468,-0.689843710920692));
#3734=CARTESIAN_POINT('Ctrl Pts',(-11.6846649679798,5.88833113237632,-0.667169129453078));
#3735=CARTESIAN_POINT('Ctrl Pts',(-11.6638747133822,5.89088291055031,-0.643210366431919));
#3736=CARTESIAN_POINT('Ctrl Pts',(-11.6441426510202,5.89340475457111,-0.618116196909614));
#3737=CARTESIAN_POINT('Ctrl Pts',(-11.6254120599292,5.8957986061758,-0.594295644375904));
#3738=CARTESIAN_POINT('Ctrl Pts',(-11.6076352765853,5.89816548504561,-0.569452789017778));
#3739=CARTESIAN_POINT('Ctrl Pts',(-11.590985695849,5.90045750206494,-0.543755474004179));
#3740=CARTESIAN_POINT('Ctrl Pts',(-11.5743648229732,5.90274556709859,-0.51810246730951));
#3741=CARTESIAN_POINT('Ctrl Pts',(-11.5588677091084,5.90495902821867,-0.491598471425702));
#3742=CARTESIAN_POINT('Ctrl Pts',(-11.5446263223345,5.90705024359962,-0.464442891940597));
#3743=CARTESIAN_POINT('Ctrl Pts',(-11.5303801053463,5.90914216825267,-0.437278102167764));
#3744=CARTESIAN_POINT('Ctrl Pts',(-11.5173907847708,5.91111176422898,-0.409461898920433));
#3745=CARTESIAN_POINT('Ctrl Pts',(-11.5057441424055,5.91291134121083,-0.381217811782318));
#3746=CARTESIAN_POINT('Ctrl Pts',(-11.5038371418876,5.91320600074693,-0.376593175160707));
#3747=CARTESIAN_POINT('Ctrl Pts',(-11.5019660327003,5.91349610203886,-0.371957106866477));
#3748=CARTESIAN_POINT('Ctrl Pts',(-11.5001310654575,5.91378143573301,-0.367310631047959));
#3749=CARTESIAN_POINT('Ctrl Pts',(-11.4853063383237,5.91608665081212,-0.32977168510081));
#3750=CARTESIAN_POINT('Ctrl Pts',(-11.4728396786202,5.91808068251128,-0.291540832281319));
#3751=CARTESIAN_POINT('Ctrl Pts',(-11.4627498179488,5.91971698624287,-0.252949145837491));
#3752=CARTESIAN_POINT('Ctrl Pts',(-11.4567469422105,5.92069049106031,-0.229989354240704));
#3753=CARTESIAN_POINT('Ctrl Pts',(-11.4515843367821,5.92153737618263,-0.206901800000682));
#3754=CARTESIAN_POINT('Ctrl Pts',(-11.4472572995214,5.92224784012799,-0.183754896369219));
#3755=CARTESIAN_POINT('Ctrl Pts',(-11.4432489878082,5.9229059719587,-0.162312972170666));
#3756=CARTESIAN_POINT('Ctrl Pts',(-11.439961640438,5.92344703975218,-0.140819734786591));
#3757=CARTESIAN_POINT('Ctrl Pts',(-11.4373971326886,5.92387645133334,-0.119516113420817));
#3758=CARTESIAN_POINT('Ctrl Pts',(-11.4362507877717,5.92406839997666,-0.109993311990914));
#3759=CARTESIAN_POINT('Ctrl Pts',(-11.435248171785,5.92423803831645,-0.100508449595123));
#3760=CARTESIAN_POINT('Ctrl Pts',(-11.4343860977113,5.92438584936314,-0.0910830923183082));
#3761=CARTESIAN_POINT('Ctrl Pts',(-11.4327073810137,5.92467368178929,-0.0727290956907958));
#3762=CARTESIAN_POINT('Ctrl Pts',(-11.4315567599486,5.92487874563008,-0.0546031136597995));
#3763=CARTESIAN_POINT('Ctrl Pts',(-11.4308953682944,5.92499615025902,-0.0364898004670366));
#3764=CARTESIAN_POINT('Ctrl Pts',(-11.4304572876631,5.92507391461186,-0.0244922319640955));
#3765=CARTESIAN_POINT('Ctrl Pts',(-11.4302349158949,5.92511322082742,-0.0125000346912251));
#3766=CARTESIAN_POINT('Ctrl Pts',(-11.4302294949532,5.92511264772102,-0.000449864268245586));
#3767=CARTESIAN_POINT('Ctrl Pts',(-11.4302143732044,5.92511104903731,0.0331641574895805));
#3768=CARTESIAN_POINT('Ctrl Pts',(-11.4318977520128,5.9247991356592,0.067213468042801));
#3769=CARTESIAN_POINT('Ctrl Pts',(-11.4353878553072,5.92419264473191,0.101441181777182));
#3770=CARTESIAN_POINT('Ctrl Pts',(-11.4388626723955,5.92358881015732,0.135518982502963));
#3771=CARTESIAN_POINT('Ctrl Pts',(-11.4441286896916,5.92269297280656,0.169773014320252));
#3772=CARTESIAN_POINT('Ctrl Pts',(-11.4512443561658,5.92152066394918,0.203932087122808));
#3773=CARTESIAN_POINT('Ctrl Pts',(-11.4583297414214,5.92035334393449,0.237945793591238));
#3774=CARTESIAN_POINT('Ctrl Pts',(-11.467249192492,5.91891190049415,0.271864682626153));
#3775=CARTESIAN_POINT('Ctrl Pts',(-11.4780094169704,5.91721166745705,0.305413024926134));
#3776=CARTESIAN_POINT('Ctrl Pts',(-11.4846501746176,5.91616235518983,0.326117649734809));
#3777=CARTESIAN_POINT('Ctrl Pts',(-11.4919910334845,5.91501447413545,0.346681019744403));
#3778=CARTESIAN_POINT('Ctrl Pts',(-11.5000236454424,5.91377162874814,0.367038507229061));
#3779=CARTESIAN_POINT('Ctrl Pts',(-11.5110521468223,5.91206524455569,0.394988641007747));
#3780=CARTESIAN_POINT('Ctrl Pts',(-11.5233988641988,5.91017984926752,0.422578110632233));
#3781=CARTESIAN_POINT('Ctrl Pts',(-11.5369898164793,5.90816323008511,0.449580979993369));
#3782=CARTESIAN_POINT('Ctrl Pts',(-11.5505815991783,5.90614648768562,0.476585499252034));
#3783=CARTESIAN_POINT('Ctrl Pts',(-11.5654174905502,5.90399850535563,0.503002719000625));
#3784=CARTESIAN_POINT('Ctrl Pts',(-11.5813761495079,5.90176707905666,0.528628574440787));
#3785=CARTESIAN_POINT('Ctrl Pts',(-11.5973542760978,5.89953293068769,0.554285690322862));
#3786=CARTESIAN_POINT('Ctrl Pts',(-11.6144574953387,5.8972151346425,0.579148962563932));
#3787=CARTESIAN_POINT('Ctrl Pts',(-11.6325217821314,5.89486166201193,0.603044414900698));
#3788=CARTESIAN_POINT('Ctrl Pts',(-11.6506773225831,5.89249630056497,0.627060577647201));
#3789=CARTESIAN_POINT('Ctrl Pts',(-11.6698031472941,5.89009490117412,0.650098664204443));
#3790=CARTESIAN_POINT('Ctrl Pts',(-11.689697113958,5.88770616560203,0.672020790277225));
#3791=CARTESIAN_POINT('Ctrl Pts',(-11.695162664264,5.88704989857104,0.678043545059696));
#3792=CARTESIAN_POINT('Ctrl Pts',(-11.700686012957,5.88639458738996,0.683982313641876));
#3793=CARTESIAN_POINT('Ctrl Pts',(-11.7062625862806,5.88574124196773,0.689834807516864));
#3794=CARTESIAN_POINT('Ctrl Pts',(-11.7263477798429,5.88338808197015,0.710913786574672));
#3795=CARTESIAN_POINT('Ctrl Pts',(-11.7477609028786,5.88098567143924,0.731537493965504));
#3796=CARTESIAN_POINT('Ctrl Pts',(-11.770433452944,5.87858424746972,0.751444819316098));
#3797=CARTESIAN_POINT('Ctrl Pts',(-11.7928148101204,5.87621366597628,0.771096466696523));
#3798=CARTESIAN_POINT('Ctrl Pts',(-11.8164232274,5.87384404586535,0.7900493849918));
#3799=CARTESIAN_POINT('Ctrl Pts',(-11.8411460208529,5.87152371333848,0.808072261471275));
#3800=CARTESIAN_POINT('Ctrl Pts',(-11.8657285654887,5.86921654372107,0.825992896789759));
#3801=CARTESIAN_POINT('Ctrl Pts',(-11.8914125449874,5.86695810407126,0.842993422903399));
#3802=CARTESIAN_POINT('Ctrl Pts',(-11.9180447110984,5.8647959028048,0.858875340688263));
#3803=CARTESIAN_POINT('Ctrl Pts',(-11.9445485982909,5.86264411619401,0.874680760180534));
#3804=CARTESIAN_POINT('Ctrl Pts',(-11.9719910902365,5.86058764309823,0.889377824348961));
#3805=CARTESIAN_POINT('Ctrl Pts',(-12.0001849714123,5.85867330873447,0.902807728591163));
#3806=CARTESIAN_POINT('Ctrl Pts',(-12.0104845902071,5.85797397563912,0.907713860289824));
#3807=CARTESIAN_POINT('Ctrl Pts',(-12.0208841714127,5.85729361156878,0.91245127650592));
#3808=CARTESIAN_POINT('Ctrl Pts',(-12.0313735835027,5.85663449938017,0.91701365454424));
#3809=CARTESIAN_POINT('Ctrl Pts',(-12.0589221689359,5.85490345780396,0.928995933444965));
#3810=CARTESIAN_POINT('Ctrl Pts',(-12.0871215827979,5.85333759236008,0.939780299010638));
#3811=CARTESIAN_POINT('Ctrl Pts',(-12.1157570467819,5.85194708130452,0.949266634293753));
#3812=CARTESIAN_POINT('Ctrl Pts',(-12.1444268796063,5.85055490133058,0.958764355260822));
#3813=CARTESIAN_POINT('Ctrl Pts',(-12.1735331620478,5.84933849692505,0.966960697313565));
#3814=CARTESIAN_POINT('Ctrl Pts',(-12.2028436425206,5.84830808303634,0.973804764894563));
#3815=CARTESIAN_POINT('Ctrl Pts',(-12.2322083633487,5.84727576232065,0.98066149772876));
#3816=CARTESIAN_POINT('Ctrl Pts',(-12.261777353607,5.84643012112625,0.986160875941255));
#3817=CARTESIAN_POINT('Ctrl Pts',(-12.2913103809521,5.84578143121621,0.990303745261672));
#3818=CARTESIAN_POINT('Ctrl Pts',(-12.3210469485782,5.84512827056483,0.994475167048973));
#3819=CARTESIAN_POINT('Ctrl Pts',(-12.3507463670084,5.8446747853114,0.997271376916708));
#3820=CARTESIAN_POINT('Ctrl Pts',(-12.3801670394779,5.84443146106362,0.998746094201777));
#3821=CARTESIAN_POINT('Ctrl Pts',(-12.3969595494538,5.84429257828103,0.999587822233208));
#3822=CARTESIAN_POINT('Ctrl Pts',(-12.4136613750755,5.84422216200635,0.999999999999999));
#3823=CARTESIAN_POINT('Ctrl Pts',(-12.4302293937643,5.84422216200635,0.999999999999999));
#3824=CARTESIAN_POINT('Origin',(-12.4302293937643,0.,0.));
#3825=CARTESIAN_POINT('',(-13.4302293937643,4.5,-6.73555739531044E-16));
#3826=CARTESIAN_POINT('Origin',(-12.4302293937643,4.5,-5.51091059616309E-16));
#3827=CARTESIAN_POINT('',(-13.4302293937643,1.49975978266185E-32,1.22464679914735E-16));
#3828=CARTESIAN_POINT('Ctrl Pts',(-12.4302293937643,1.29489435381091,-6.0889402328518));
#3829=CARTESIAN_POINT('Ctrl Pts',(-12.5942565650519,1.29489432255619,-6.08894022144968));
#3830=CARTESIAN_POINT('Ctrl Pts',(-12.9434847664517,1.22941870144897,-6.10373432775123));
#3831=CARTESIAN_POINT('Ctrl Pts',(-13.2352135646621,1.03138926022157,-6.14034164499865));
#3832=CARTESIAN_POINT('Ctrl Pts',(-13.4649707254284,0.802539126833306,-6.17429853801347));
#3833=CARTESIAN_POINT('Ctrl Pts',(-13.6645538759468,0.510108161031878,-6.21087860035388));
#3834=CARTESIAN_POINT('Ctrl Pts',(-13.7382347656975,0.121768500013446,-6.2270006516547));
#3835=CARTESIAN_POINT('Ctrl Pts',(-13.722307002809,-0.206473102178789,-6.22359662674633));
#3836=CARTESIAN_POINT('Ctrl Pts',(-13.639475073467,-0.54967950795853,-6.20621767344192));
#3837=CARTESIAN_POINT('Ctrl Pts',(-13.4650599641877,-0.802298136921999,
-6.17429031658926));
#3838=CARTESIAN_POINT('Ctrl Pts',(-13.2351717858284,-1.03178961021895,-6.14014988493062));
#3839=CARTESIAN_POINT('Ctrl Pts',(-13.0895235534449,-1.13087278981698,-6.12193678986932));
#3840=CARTESIAN_POINT('Ctrl Pts',(-12.8085826603911,-1.24610737129426,-6.09931038796544));
#3841=CARTESIAN_POINT('Ctrl Pts',(-12.5543859913687,-1.30578995791277,-6.08658018368838));
#3842=CARTESIAN_POINT('Ctrl Pts',(-12.0552211457951,-1.28477538936707,-6.09114347875703));
#3843=CARTESIAN_POINT('Ctrl Pts',(-11.6810858915091,-1.09012014643369,-6.13128471453802));
#3844=CARTESIAN_POINT('Ctrl Pts',(-11.4246965219914,-0.830211081602218,
-6.16997769478043));
#3845=CARTESIAN_POINT('Ctrl Pts',(-11.2673613307636,-0.624855866522035,
-6.19690899075049));
#3846=CARTESIAN_POINT('Ctrl Pts',(-11.0920011380406,-0.125799266344306,
-6.23306766503593));
#3847=CARTESIAN_POINT('Ctrl Pts',(-11.1298693974023,0.254022871674497,-6.22462921167978));
#3848=CARTESIAN_POINT('Ctrl Pts',(-11.2951627568963,0.657046732135944,-6.19244771333686));
#3849=CARTESIAN_POINT('Ctrl Pts',(-11.3950769811324,0.801381093653546,-6.17436843941782));
#3850=CARTESIAN_POINT('Ctrl Pts',(-11.6251524041765,1.03086438702109,-6.14021337372633));
#3851=CARTESIAN_POINT('Ctrl Pts',(-11.7709112212583,1.13013251926196,-6.12202566624175));
#3852=CARTESIAN_POINT('Ctrl Pts',(-12.0914404061413,1.26217657193465,-6.09612077171828));
#3853=CARTESIAN_POINT('Ctrl Pts',(-12.2662022355639,1.29489435617836,-6.08894022430558));
#3854=CARTESIAN_POINT('Ctrl Pts',(-12.4302293937643,1.29489435381091,-6.0889402328518));
#3855=CARTESIAN_POINT('Ctrl Pts',(-12.4302293937643,1.19652398778682,-6.00730758749701));
#3856=CARTESIAN_POINT('Ctrl Pts',(-12.5835260128158,1.19660554925645,-6.00733734217367));
#3857=CARTESIAN_POINT('Ctrl Pts',(-12.9099794791603,1.1339456710644,-6.02027410479885));
#3858=CARTESIAN_POINT('Ctrl Pts',(-13.1793649483868,0.947760265143857,-6.05208309125148));
#3859=CARTESIAN_POINT('Ctrl Pts',(-13.390127239501,0.734644744099366,-6.08145723820567));
#3860=CARTESIAN_POINT('Ctrl Pts',(-13.5712908603111,0.464550273602845,-6.11289252680422));
#3861=CARTESIAN_POINT('Ctrl Pts',(-13.6372762454486,0.110863463753234,-6.12664471204441));
#3862=CARTESIAN_POINT('Ctrl Pts',(-13.6230233985846,-0.188078828642945,
-6.12375264534608));
#3863=CARTESIAN_POINT('Ctrl Pts',(-13.5485622985786,-0.501106347863059,
-6.10889585516032));
#3864=CARTESIAN_POINT('Ctrl Pts',(-13.3901851790633,-0.734519663395452,
-6.08143345776283));
#3865=CARTESIAN_POINT('Ctrl Pts',(-13.1793404196312,-0.948112795692235,
-6.05190225429682));
#3866=CARTESIAN_POINT('Ctrl Pts',(-13.0448314929934,-1.04131898524137,-6.03606502647125));
#3867=CARTESIAN_POINT('Ctrl Pts',(-12.7836826024607,-1.15012783687734,-6.0163867285));
#3868=CARTESIAN_POINT('Ctrl Pts',(-12.5464205975656,-1.20689836538162,-6.00524419490769));
#3869=CARTESIAN_POINT('Ctrl Pts',(-12.0794526073123,-1.18675056022211,-6.00927493048454));
#3870=CARTESIAN_POINT('Ctrl Pts',(-11.7321555677729,-1.00228782075479,-6.04426997438495));
#3871=CARTESIAN_POINT('Ctrl Pts',(-11.4971890642621,-0.760513752850325,
-6.07766139091982));
#3872=CARTESIAN_POINT('Ctrl Pts',(-11.3537752566932,-0.570286282304659,
-6.10091025389764));
#3873=CARTESIAN_POINT('Ctrl Pts',(-11.1959278067123,-0.113851829768248,
-6.1318171205129));
#3874=CARTESIAN_POINT('Ctrl Pts',(-11.2298363795958,0.230967119360158,-6.12460974003898));
#3875=CARTESIAN_POINT('Ctrl Pts',(-11.3791293387795,0.600065235007544,-6.09708188247935));
#3876=CARTESIAN_POINT('Ctrl Pts',(-11.4699934418307,0.733649918402728,-6.08148733752786));
#3877=CARTESIAN_POINT('Ctrl Pts',(-11.6809686581905,0.947165898685803,-6.0519761018612));
#3878=CARTESIAN_POINT('Ctrl Pts',(-11.8155823945189,1.04056140059047,-6.03616052651344));
#3879=CARTESIAN_POINT('Ctrl Pts',(-12.1135732968508,1.16533663101808,-6.01359382211873));
#3880=CARTESIAN_POINT('Ctrl Pts',(-12.2768986229754,1.19651780974642,-6.00732988949686));
#3881=CARTESIAN_POINT('Ctrl Pts',(-12.4302293937643,1.19652398778682,-6.00730758749701));
#3882=CARTESIAN_POINT('Ctrl Pts',(-12.4302293937643,1.09815362176272,-5.92567494214221));
#3883=CARTESIAN_POINT('Ctrl Pts',(-12.5728768111359,1.09807191176829,-5.92564513328179));
#3884=CARTESIAN_POINT('Ctrl Pts',(-12.8764400238043,1.03857307634312,-5.93677323915331));
#3885=CARTESIAN_POINT('Ctrl Pts',(-13.1236421530229,0.863834068887647,-5.9638111997203));
#3886=CARTESIAN_POINT('Ctrl Pts',(-13.3152938488915,0.666818346565923,-5.98856002821125));
#3887=CARTESIAN_POINT('Ctrl Pts',(-13.4781043169547,0.419015044302822,-6.01490064545119));
#3888=CARTESIAN_POINT('Ctrl Pts',(-13.5363318958501,0.0999234953363876,
-6.02625541555216));
#3889=CARTESIAN_POINT('Ctrl Pts',(-13.5236242325651,-0.169584645174253,
-6.02383257520469));
#3890=CARTESIAN_POINT('Ctrl Pts',(-13.45763379556,-0.452598972368938,-6.011534802412));
#3891=CARTESIAN_POINT('Ctrl Pts',(-13.3153133841291,-0.666694064607999,
-5.98855204897587));
#3892=CARTESIAN_POINT('Ctrl Pts',(-13.1235487664965,-0.864416414698098,
-5.96366385619052));
#3893=CARTESIAN_POINT('Ctrl Pts',(-13.0002703379808,-0.951649292171483,
-5.95024248073981));
#3894=CARTESIAN_POINT('Ctrl Pts',(-12.7587075542712,-1.05425776004711,-5.93340511818793));
#3895=CARTESIAN_POINT('Ctrl Pts',(-12.5386313682688,-1.10804595290956,-5.92389983389524));
#3896=CARTESIAN_POINT('Ctrl Pts',(-12.1032856759994,-1.08903105885641,-5.92731281534742));
#3897=CARTESIAN_POINT('Ctrl Pts',(-11.7831058258753,-0.914801975659288,
-5.95717971506951));
#3898=CARTESIAN_POINT('Ctrl Pts',(-11.5695163116143,-0.690787431055235,
-5.98544778843915));
#3899=CARTESIAN_POINT('Ctrl Pts',(-11.4400693088082,-0.515889562697353,
-6.00490223026015));
#3900=CARTESIAN_POINT('Ctrl Pts',(-11.2997931554053,-0.101999726766142,
-6.03060418648155));
#3901=CARTESIAN_POINT('Ctrl Pts',(-11.3296621227584,0.20759284922966,-6.02466259409955));
#3902=CARTESIAN_POINT('Ctrl Pts',(-11.4632375981302,0.543731219297565,-6.0016238831943));
#3903=CARTESIAN_POINT('Ctrl Pts',(-11.5448774670807,0.665911891095343,-5.98861915101148));
#3904=CARTESIAN_POINT('Ctrl Pts',(-11.7368656075404,0.863751696770123,-5.96368471390795));
#3905=CARTESIAN_POINT('Ctrl Pts',(-11.8602650367562,0.951079271006522,-5.95028481323786));
#3906=CARTESIAN_POINT('Ctrl Pts',(-12.1357219210113,1.06855012001856,-5.93104620471383));
#3907=CARTESIAN_POINT('Ctrl Pts',(-12.2876161903209,1.09815981105343,-5.92565259953004));
#3908=CARTESIAN_POINT('Ctrl Pts',(-12.4302293937643,1.09815362176272,-5.92567494214221));
#3909=CARTESIAN_POINT('Ctrl Pts',(-12.4302293937643,0.99978325573863,-5.84404229678742));
#3910=CARTESIAN_POINT('Ctrl Pts',(-12.5621461601267,0.99978343577442,-5.8440423624668));
#3911=CARTESIAN_POINT('Ctrl Pts',(-12.8429347779986,0.943099924012935,-5.85331306554794));
#3912=CARTESIAN_POINT('Ctrl Pts',(-13.0677933839801,0.780205434661611,-5.87555266216742));
#3913=CARTESIAN_POINT('Ctrl Pts',(-13.2404503507067,0.598923881286639,-5.89571879628772));
#3914=CARTESIAN_POINT('Ctrl Pts',(-13.3848412084689,0.373457129363051,-5.91691457895316));
#3915=CARTESIAN_POINT('Ctrl Pts',(-13.4353733583957,0.0890185014896255,
-5.92589951644267));
#3916=CARTESIAN_POINT('Ctrl Pts',(-13.424340768652,-0.15119049294569,-5.92398868618882));
#3917=CARTESIAN_POINT('Ctrl Pts',(-13.3667210397683,-0.404025732400016,
-5.91421303176758));
#3918=CARTESIAN_POINT('Ctrl Pts',(-13.2404385953741,-0.59891564829936,-5.89569521995717));
#3919=CARTESIAN_POINT('Ctrl Pts',(-13.067717352081,-0.78073962392833,-5.8754162143469));
#3920=CARTESIAN_POINT('Ctrl Pts',(-12.9555781185883,-0.862095628303779,
-5.8643706575833));
#3921=CARTESIAN_POINT('Ctrl Pts',(-12.7338075873915,-0.958278092730466,
-5.85048152908445));
#3922=CARTESIAN_POINT('Ctrl Pts',(-12.5306657605727,-1.00915431280731,-5.84256385527983));
#3923=CARTESIAN_POINT('Ctrl Pts',(-12.1275176212317,-0.991005858992733,
-5.84544438068066));
#3924=CARTESIAN_POINT('Ctrl Pts',(-11.8341756471326,-0.82696922929531,-5.87016506660928));
#3925=CARTESIAN_POINT('Ctrl Pts',(-11.6420090545806,-0.621090137505721,
-5.89313135988199));
#3926=CARTESIAN_POINT('Ctrl Pts',(-11.5264833802844,-0.461319768593579,
-5.90890350468299));
#3927=CARTESIAN_POINT('Ctrl Pts',(-11.4037198985297,-0.0900521744392636,
-5.92935359629313));
#3928=CARTESIAN_POINT('Ctrl Pts',(-11.4296292764396,0.184537483648944,-5.92464303464332));
#3929=CARTESIAN_POINT('Ctrl Pts',(-11.5472040079934,0.486748936019,-5.9062581642446));
#3930=CARTESIAN_POINT('Ctrl Pts',(-11.6197939671611,0.598180724164063,-5.89573803344012));
#3931=CARTESIAN_POINT('Ctrl Pts',(-11.7926817635769,0.780052863263822,-5.87544750774877));
#3932=CARTESIAN_POINT('Ctrl Pts',(-11.9049361960917,0.861508044287461,-5.86441968634761));
#3933=CARTESIAN_POINT('Ctrl Pts',(-12.1578547926178,0.971710114229192,-5.84851928020843));
#3934=CARTESIAN_POINT('Ctrl Pts',(-12.2983125520166,0.999783242101451,-5.84404234601604));
#3935=CARTESIAN_POINT('Ctrl Pts',(-12.4302293937643,0.99978325573863,-5.84404229678742));
#3936=CARTESIAN_POINT('',(-12.4302293937643,1.,-5.84422216200635));
#3937=CARTESIAN_POINT('',(-12.4302293937643,1.29485665783831,-6.08890895085005));
#3938=CARTESIAN_POINT('',(-13.4302291165819,-0.00074455678695871,-5.92515607096498));
#3939=CARTESIAN_POINT('Ctrl Pts',(-12.4302293937643,1.,-5.84422216200635));
#3940=CARTESIAN_POINT('Ctrl Pts',(-12.5068876215205,1.,-5.84422216200635));
#3941=CARTESIAN_POINT('Ctrl Pts',(-12.583514447768,0.991164337845293,-5.84618803600395));
#3942=CARTESIAN_POINT('Ctrl Pts',(-12.734482852694,0.955797513292997,-5.85160509572529));
#3943=CARTESIAN_POINT('Ctrl Pts',(-12.8081512123687,0.92914750024174,-5.85522477680349));
#3944=CARTESIAN_POINT('Ctrl Pts',(-12.9239247195674,0.871137085216352,-5.86352598326324));
#3945=CARTESIAN_POINT('Ctrl Pts',(-12.9678164063148,0.844756284210404,-5.86723138398402));
#3946=CARTESIAN_POINT('Ctrl Pts',(-13.0616660207753,0.778065357329548,-5.87582109133897));
#3947=CARTESIAN_POINT('Ctrl Pts',(-13.1101602808476,0.736060124110439,-5.88069567821875));
#3948=CARTESIAN_POINT('Ctrl Pts',(-13.2147331458838,0.626288084301812,-5.89292243393707));
#3949=CARTESIAN_POINT('Ctrl Pts',(-13.26672687916,0.554987202036906,-5.90053924283666));
#3950=CARTESIAN_POINT('Ctrl Pts',(-13.329015288876,0.440435511458002,-5.90951215353627));
#3951=CARTESIAN_POINT('Ctrl Pts',(-13.3468856793851,0.401923730048892,-5.91211175363263));
#3952=CARTESIAN_POINT('Ctrl Pts',(-13.3850158785098,0.303849355425613,-5.91790597801221));
#3953=CARTESIAN_POINT('Ctrl Pts',(-13.4022161136297,0.243296810883259,-5.92076752333631));
#3954=CARTESIAN_POINT('Ctrl Pts',(-13.4247157097056,0.12137679578229,-5.9244956146738));
#3955=CARTESIAN_POINT('Ctrl Pts',(-13.4302746508587,0.0604058320419782,
-5.92539504948499));
#3956=CARTESIAN_POINT('Ctrl Pts',(-13.4302291165292,-0.00074462755025776,
-5.92532717514869));
#3957=CARTESIAN_POINT('Ctrl Pts',(-13.4302291165819,-0.00074455678695871,
-5.92515607096498));
#3958=CARTESIAN_POINT('Ctrl Pts',(-13.4302145007545,-0.0203747898610464,
-5.92516162275695));
#3959=CARTESIAN_POINT('Ctrl Pts',(-13.4296263010912,-0.0398710445290823,
-5.92506363544977));
#3960=CARTESIAN_POINT('Ctrl Pts',(-13.4284619148531,-0.0594292338889376,
-5.9248625596374));
#3961=CARTESIAN_POINT('Ctrl Pts',(-13.427825762458,-0.0701146822394427,
-5.92475270359868));
#3962=CARTESIAN_POINT('Ctrl Pts',(-13.4270167202947,-0.0808186195238017,
-5.92461207678402));
#3963=CARTESIAN_POINT('Ctrl Pts',(-13.4260278070042,-0.0915724859817269,
-5.92444075267486));
#3964=CARTESIAN_POINT('Ctrl Pts',(-13.4234433178898,-0.119677326989046,
-5.92399300331256));
#3965=CARTESIAN_POINT('Ctrl Pts',(-13.4196244803128,-0.148112331845129,
-5.9233355854986));
#3966=CARTESIAN_POINT('Ctrl Pts',(-13.4145053388056,-0.176637663064945,
-5.92247964262467));
#3967=CARTESIAN_POINT('Ctrl Pts',(-13.4094168909871,-0.204991960208965,
-5.92162883186987));
#3968=CARTESIAN_POINT('Ctrl Pts',(-13.4030435605191,-0.233434848039028,
-5.92058186957752));
#3969=CARTESIAN_POINT('Ctrl Pts',(-13.3953716865626,-0.261725724093029,
-5.91934969989586));
#3970=CARTESIAN_POINT('Ctrl Pts',(-13.3877346584708,-0.289888102201762,
-5.91812312676315));
#3971=CARTESIAN_POINT('Ctrl Pts',(-13.3788108949432,-0.317899175506962,
-5.91671302485451));
#3972=CARTESIAN_POINT('Ctrl Pts',(-13.3686383796453,-0.345526518834328,
-5.91513018986864));
#3973=CARTESIAN_POINT('Ctrl Pts',(-13.3659090692588,-0.352939001675285,
-5.91470551142476));
#3974=CARTESIAN_POINT('Ctrl Pts',(-13.363090150361,-0.360323920078094,-5.91426839858579));
#3975=CARTESIAN_POINT('Ctrl Pts',(-13.3601829769247,-0.367676941304649,
-5.91381905986056));
#3976=CARTESIAN_POINT('Ctrl Pts',(-13.348323638179,-0.397672389268568,-5.91198605599245));
#3977=CARTESIAN_POINT('Ctrl Pts',(-13.3349765249106,-0.427174288976912,
-5.90994960131782));
#3978=CARTESIAN_POINT('Ctrl Pts',(-13.3202356031391,-0.455948404180037,
-5.90776747673239));
#3979=CARTESIAN_POINT('Ctrl Pts',(-13.3055877002079,-0.484540947642264,
-5.90559912188955));
#3980=CARTESIAN_POINT('Ctrl Pts',(-13.289563906132,-0.512414264265203,-5.90328692976136));
#3981=CARTESIAN_POINT('Ctrl Pts',(-13.2723027529233,-0.539363011148032,
-5.90088759429642));
#3982=CARTESIAN_POINT('Ctrl Pts',(-13.254877178999,-0.566568457695916,-5.898465404017));
#3983=CARTESIAN_POINT('Ctrl Pts',(-13.2361909738944,-0.592831045617222,
-5.89595440233023));
#3984=CARTESIAN_POINT('Ctrl Pts',(-13.2164282067282,-0.617973645468872,
-5.89341291877673));
#3985=CARTESIAN_POINT('Ctrl Pts',(-13.1966654395621,-0.643116245320522,
-5.89087143522323));
#3986=CARTESIAN_POINT('Ctrl Pts',(-13.1758267003413,-0.667138450433701,
-5.888299469803));
#3987=CARTESIAN_POINT('Ctrl Pts',(-13.1541297156023,-0.689904576041336,
-5.88575535205665));
#3988=CARTESIAN_POINT('Ctrl Pts',(-13.1337114574319,-0.711328964535441,
-5.8833611736219));
#3989=CARTESIAN_POINT('Ctrl Pts',(-13.1119354995351,-0.732268036614787,
-5.88091652810431));
#3990=CARTESIAN_POINT('Ctrl Pts',(-13.0888693452294,-0.752458247568669,
-5.87847421176537));
#3991=CARTESIAN_POINT('Ctrl Pts',(-13.0660882115552,-0.772398974945793,
-5.87606207429961));
#3992=CARTESIAN_POINT('Ctrl Pts',(-13.0420487837158,-0.791608598781269,
-5.87365220880638));
#3993=CARTESIAN_POINT('Ctrl Pts',(-13.0168632956008,-0.809852249003558,
-5.87129547847511));
#3994=CARTESIAN_POINT('Ctrl Pts',(-12.9918183626218,-0.827994085088781,
-5.8689519005811));
#3995=CARTESIAN_POINT('Ctrl Pts',(-12.9656404510038,-0.845180103433922,
-5.86666086643067));
#3996=CARTESIAN_POINT('Ctrl Pts',(-12.9384829388873,-0.861207485957893,
-5.86447239238519));
#3997=CARTESIAN_POINT('Ctrl Pts',(-12.9114573425185,-0.877157016573312,
-5.86229454870192));
#3998=CARTESIAN_POINT('Ctrl Pts',(-12.8834621017052,-0.891958633552042,
-5.86021827118614));
#3999=CARTESIAN_POINT('Ctrl Pts',(-12.8546851894651,-0.905448660883642,
-5.85829285088076));
#4000=CARTESIAN_POINT('Ctrl Pts',(-12.8461436459829,-0.909452761603969,
-5.85772134893771));
#4001=CARTESIAN_POINT('Ctrl Pts',(-12.8375334567298,-0.913341579410674,
-5.85716313777255));
#4002=CARTESIAN_POINT('Ctrl Pts',(-12.8288600642316,-0.917111546412302,
-5.85661950636029));
#4003=CARTESIAN_POINT('Ctrl Pts',(-12.7961359807478,-0.931335359633967,
-5.85456842430408));
#4004=CARTESIAN_POINT('Ctrl Pts',(-12.7626532281845,-0.943801826616426,
-5.85275395442562));
#4005=CARTESIAN_POINT('Ctrl Pts',(-12.7286738356243,-0.954427008797875,
-5.85119022535545));
#4006=CARTESIAN_POINT('Ctrl Pts',(-12.6946247640078,-0.965073979263702,
-5.84962328966039));
#4007=CARTESIAN_POINT('Ctrl Pts',(-12.6600776972981,-0.973871960195361,
-5.84830812417968));
#4008=CARTESIAN_POINT('Ctrl Pts',(-12.6253069014017,-0.980787829254606,
-5.84725894463988));
#4009=CARTESIAN_POINT('Ctrl Pts',(-12.5940277649148,-0.98700921149949,-5.84631512298786));
#4010=CARTESIAN_POINT('Ctrl Pts',(-12.5625680645456,-0.991708188398394,
-5.84558654923866));
#4011=CARTESIAN_POINT('Ctrl Pts',(-12.531127836805,-0.994896730415759,-5.84508357217886));
#4012=CARTESIAN_POINT('Ctrl Pts',(-12.4973809048887,-0.998319209135062,
-5.84454369273739));
#4013=CARTESIAN_POINT('Ctrl Pts',(-12.4636986156402,-1.00000481725209,-5.8442637274595));
#4014=CARTESIAN_POINT('Ctrl Pts',(-12.4300857711154,-0.999999989686268,
-5.8442498696352));
#4015=CARTESIAN_POINT('Ctrl Pts',(-12.3964457198719,-0.999995158212949,
-5.84423600059418));
#4016=CARTESIAN_POINT('Ctrl Pts',(-12.3628741784227,-0.998297160738039,
-5.84448866996346));
#4017=CARTESIAN_POINT('Ctrl Pts',(-12.3293717699161,-0.994900869288844,
-5.84501408608402));
#4018=CARTESIAN_POINT('Ctrl Pts',(-12.2958961260104,-0.991507291088906,
-5.84553908245706));
#4019=CARTESIAN_POINT('Ctrl Pts',(-12.2624884600473,-0.98641801752302,-5.8463363899684));
#4020=CARTESIAN_POINT('Ctrl Pts',(-12.2291608584518,-0.979577176187413,
-5.84741220209162));
#4021=CARTESIAN_POINT('Ctrl Pts',(-12.2003045415045,-0.973654113131077,
-5.84834368152961));
#4022=CARTESIAN_POINT('Ctrl Pts',(-12.1714822894461,-0.966404873720001,
-5.84948394922433));
#4023=CARTESIAN_POINT('Ctrl Pts',(-12.1429321226033,-0.957841468085098,
-5.85079937270242));
#4024=CARTESIAN_POINT('Ctrl Pts',(-12.1144345913459,-0.949293850094169,
-5.85211237104285));
#4025=CARTESIAN_POINT('Ctrl Pts',(-12.0862088137393,-0.939437011609988,
-5.85359987992147));
#4026=CARTESIAN_POINT('Ctrl Pts',(-12.0584819453244,-0.928333902525599,
-5.85522845253844));
#4027=CARTESIAN_POINT('Ctrl Pts',(-12.0307493255855,-0.917228490347451,
-5.85685736296667));
#4028=CARTESIAN_POINT('Ctrl Pts',(-12.0035164563319,-0.904876542764548,
-5.8586273956604));
#4029=CARTESIAN_POINT('Ctrl Pts',(-11.976991236791,-0.891389462055422,-5.86050508300206));
#4030=CARTESIAN_POINT('Ctrl Pts',(-11.9503194013934,-0.877827832674227,
-5.86239314909809));
#4031=CARTESIAN_POINT('Ctrl Pts',(-11.9243636448556,-0.863118854449607,
-5.86439006323465));
#4032=CARTESIAN_POINT('Ctrl Pts',(-11.8993064649707,-0.847420110500802,
-5.86646179975291));
#4033=CARTESIAN_POINT('Ctrl Pts',(-11.8741364085495,-0.831650647506662,
-5.86854286894321));
#4034=CARTESIAN_POINT('Ctrl Pts',(-11.8498735094175,-0.814882991634751,
-5.87069943614703));
#4035=CARTESIAN_POINT('Ctrl Pts',(-11.8266657236187,-0.797314803625511,
-5.87289701379889));
#4036=CARTESIAN_POINT('Ctrl Pts',(-11.8031493349558,-0.779513004655496,
-5.875123813487));
#4037=CARTESIAN_POINT('Ctrl Pts',(-11.7807166929995,-0.760889825243683,
-5.87739272153807));
#4038=CARTESIAN_POINT('Ctrl Pts',(-11.759477199834,-0.74168153161429,-5.8796678562279));
#4039=CARTESIAN_POINT('Ctrl Pts',(-11.7407509176273,-0.724746102674908,
-5.88167378047139));
#4040=CARTESIAN_POINT('Ctrl Pts',(-11.7229515053941,-0.707356589426639,
-5.88368454497276));
#4041=CARTESIAN_POINT('Ctrl Pts',(-11.7061231638194,-0.689688457026103,
-5.88567555763584));
#4042=CARTESIAN_POINT('Ctrl Pts',(-11.6866581296135,-0.669252052166742,
-5.88797852548441));
#4043=CARTESIAN_POINT('Ctrl Pts',(-11.667818004418,-0.647733283425998,-5.89030237056838));
#4044=CARTESIAN_POINT('Ctrl Pts',(-11.649809623362,-0.625255933170801,-5.89260310173008));
#4045=CARTESIAN_POINT('Ctrl Pts',(-11.6318783158107,-0.602874783021202,
-5.89489398606472));
#4046=CARTESIAN_POINT('Ctrl Pts',(-11.6147721838589,-0.579543634374203,
-5.89716195390281));
#4047=CARTESIAN_POINT('Ctrl Pts',(-11.5986621529662,-0.555424093852063,
-5.89936357650184));
#4048=CARTESIAN_POINT('Ctrl Pts',(-11.58258732708,-0.53135726139663,-5.90156038792834));
#4049=CARTESIAN_POINT('Ctrl Pts',(-11.5675046859438,-0.506505991676054,
-5.90369114376546));
#4050=CARTESIAN_POINT('Ctrl Pts',(-11.5535435587647,-0.481063349997679,
-5.90571269936149));
#4051=CARTESIAN_POINT('Ctrl Pts',(-11.5488146310658,-0.472445391617939,
-5.90639744280163));
#4052=CARTESIAN_POINT('Ctrl Pts',(-11.5442140057291,-0.463759824048832,
-5.90706965748497));
#4053=CARTESIAN_POINT('Ctrl Pts',(-11.5397455322372,-0.45501482652746,-5.90772766671857));
#4054=CARTESIAN_POINT('Ctrl Pts',(-11.5249613802793,-0.426081596317538,
-5.9099047208103));
#4055=CARTESIAN_POINT('Ctrl Pts',(-11.5116020195662,-0.396446991709848,
-5.9119262752392));
#4056=CARTESIAN_POINT('Ctrl Pts',(-11.4997509995239,-0.366346772678213,
-5.91376075413862));
#4057=CARTESIAN_POINT('Ctrl Pts',(-11.4878540732106,-0.336129957032688,
-5.91560233910022));
#4058=CARTESIAN_POINT('Ctrl Pts',(-11.4774773723843,-0.305444596233139,
-5.91725539640872));
#4059=CARTESIAN_POINT('Ctrl Pts',(-11.4686542921061,-0.274542025691928,
-5.91868798183615));
#4060=CARTESIAN_POINT('Ctrl Pts',(-11.4600139155072,-0.244279369235048,
-5.92009090204234));
#4061=CARTESIAN_POINT('Ctrl Pts',(-11.4528632919579,-0.213809061728737,
-5.92128238665944));
#4062=CARTESIAN_POINT('Ctrl Pts',(-11.4471853155946,-0.183369409595853,
-5.92223243510267));
#4063=CARTESIAN_POINT('Ctrl Pts',(-11.4411101863144,-0.150800619216677,
-5.92324893583213));
#4064=CARTESIAN_POINT('Ctrl Pts',(-11.4367166701769,-0.118291409597998,
-5.92398904407821));
#4065=CARTESIAN_POINT('Ctrl Pts',(-11.4339211481789,-0.0858480039286165,
-5.92445833008817));
#4066=CARTESIAN_POINT('Ctrl Pts',(-11.431089721008,-0.0529879010954458,
-5.92493364352174));
#4067=CARTESIAN_POINT('Ctrl Pts',(-11.4298974125296,-0.0201943247625311,
-5.92513113326092));
#4068=CARTESIAN_POINT('Ctrl Pts',(-11.4303080569058,0.0125427307665045,
-5.92505658695115));
#4069=CARTESIAN_POINT('Ctrl Pts',(-11.4307185775025,0.0452699184545837,
-5.92498206311167));
#4070=CARTESIAN_POINT('Ctrl Pts',(-11.4327311014724,0.0779416178077606,
-5.92463566719669));
#4071=CARTESIAN_POINT('Ctrl Pts',(-11.4363609723752,0.110569258682268,-5.92402318161956));
#4072=CARTESIAN_POINT('Ctrl Pts',(-11.4399493805261,0.142824205370928,-5.92341769225201));
#4073=CARTESIAN_POINT('Ctrl Pts',(-11.4451185935596,0.175037037023386,-5.92255215740294));
#4074=CARTESIAN_POINT('Ctrl Pts',(-11.4519320204813,0.207205814174295,-5.92143216358902));
#4075=CARTESIAN_POINT('Ctrl Pts',(-11.4585455065396,0.23843059454462,-5.92034503613336));
#4076=CARTESIAN_POINT('Ctrl Pts',(-11.4667085178863,0.269614642654035,-5.91901816484915));
#4077=CARTESIAN_POINT('Ctrl Pts',(-11.4765205424234,0.300731486336286,-5.91745665873306));
#4078=CARTESIAN_POINT('Ctrl Pts',(-11.4834028145948,0.322557215218856,-5.91636139953884));
#4079=CARTESIAN_POINT('Ctrl Pts',(-11.491097239556,0.344349397393402,-5.91515070496908));
#4080=CARTESIAN_POINT('Ctrl Pts',(-11.4996492233318,0.366088167519528,-5.9138263380358));
#4081=CARTESIAN_POINT('Ctrl Pts',(-11.51159593145,0.396456179007265,-5.91197626142105));
#4082=CARTESIAN_POINT('Ctrl Pts',(-11.5250526304243,0.426287151505064,-5.90992593215957));
#4083=CARTESIAN_POINT('Ctrl Pts',(-11.539917668182,0.455351546929103,-5.90773166728562));
#4084=CARTESIAN_POINT('Ctrl Pts',(-11.5547892593215,0.484428755645817,-5.90553643505083));
#4085=CARTESIAN_POINT('Ctrl Pts',(-11.5710700779739,0.512738103043412,-5.90319714026504));
#4086=CARTESIAN_POINT('Ctrl Pts',(-11.5886129139444,0.540075643679213,-5.90077017447893));
#4087=CARTESIAN_POINT('Ctrl Pts',(-11.606228870658,0.567527130617118,-5.89833309279467));
#4088=CARTESIAN_POINT('Ctrl Pts',(-11.6251169246386,0.593998158860184,-5.89580760773948));
#4089=CARTESIAN_POINT('Ctrl Pts',(-11.6450883435803,0.619316987750228,-5.89325081894841));
#4090=CARTESIAN_POINT('Ctrl Pts',(-11.6644136094771,0.643816654094558,-5.89077675221468));
#4091=CARTESIAN_POINT('Ctrl Pts',(-11.6847525915489,0.667237341250066,-5.88827337457224));
#4092=CARTESIAN_POINT('Ctrl Pts',(-11.7059060210901,0.689460406258321,-5.88579242084807));
#4093=CARTESIAN_POINT('Ctrl Pts',(-11.7261027910912,0.710678437680429,-5.88342366775048));
#4094=CARTESIAN_POINT('Ctrl Pts',(-11.7476344282494,0.731426349304129,-5.88100685224014));
#4095=CARTESIAN_POINT('Ctrl Pts',(-11.7704316787271,0.751443261485303,-5.87859232221928));
#4096=CARTESIAN_POINT('Ctrl Pts',(-11.792944613224,0.771210532683476,-5.87620790501715));
#4097=CARTESIAN_POINT('Ctrl Pts',(-11.8166915647589,0.790264293271009,-5.87382571665301));
#4098=CARTESIAN_POINT('Ctrl Pts',(-11.8415590054149,0.808373164992864,-5.87149424468247));
#4099=CARTESIAN_POINT('Ctrl Pts',(-11.866288678916,0.826381712448536,-5.86917568921045));
#4100=CARTESIAN_POINT('Ctrl Pts',(-11.8921261252638,0.843455222096322,-5.86690728974473));
#4101=CARTESIAN_POINT('Ctrl Pts',(-11.9189171953938,0.859395040593982,-5.86473673242511));
#4102=CARTESIAN_POINT('Ctrl Pts',(-11.9455822675806,0.875259894398724,-5.86257638319934));
#4103=CARTESIAN_POINT('Ctrl Pts',(-11.9731915440691,0.890001198131698,-5.86051295798388));
#4104=CARTESIAN_POINT('Ctrl Pts',(-12.0015568587732,0.903459936989056,-5.85859347327646));
#4105=CARTESIAN_POINT('Ctrl Pts',(-12.0113696684317,0.90811590657827,-5.85792943911105));
#4106=CARTESIAN_POINT('Ctrl Pts',(-12.0212726736568,0.91261874057659,-5.85728263134725));
#4107=CARTESIAN_POINT('Ctrl Pts',(-12.0312572421975,0.916963043025268,-5.85665499654412));
#4108=CARTESIAN_POINT('Ctrl Pts',(-12.0588063180869,0.928949691958269,-5.85492324832167));
#4109=CARTESIAN_POINT('Ctrl Pts',(-12.0870049770799,0.93973768627278,-5.85335622415252));
#4110=CARTESIAN_POINT('Ctrl Pts',(-12.1156382920204,0.949227285060628,-5.85196428648677));
#4111=CARTESIAN_POINT('Ctrl Pts',(-12.1443073748145,0.958728737962493,-5.85057061005544));
#4112=CARTESIAN_POINT('Ctrl Pts',(-12.1734115519112,0.966928319492569,-5.84935245782604));
#4113=CARTESIAN_POINT('Ctrl Pts',(-12.2027184572862,0.973775525356251,-5.84832023113058));
#4114=CARTESIAN_POINT('Ctrl Pts',(-12.2320804477626,0.9806356011912,-5.84728606426737));
#4115=CARTESIAN_POINT('Ctrl Pts',(-12.2616452441127,0.986138143316237,-5.84643852252421));
#4116=CARTESIAN_POINT('Ctrl Pts',(-12.2911725495681,0.990284400605293,-5.84578806599426));
#4117=CARTESIAN_POINT('Ctrl Pts',(-12.3209050503466,0.994459471651339,-5.84513308921989));
#4118=CARTESIAN_POINT('Ctrl Pts',(-12.3505988485243,0.997259402232014,-5.84467794640146));
#4119=CARTESIAN_POINT('Ctrl Pts',(-12.3800123124227,0.998738326460704,-5.84443331722338));
#4120=CARTESIAN_POINT('Ctrl Pts',(-12.3968576798465,0.999585320276542,-5.84429321579222));
#4121=CARTESIAN_POINT('Ctrl Pts',(-12.4136112257704,1.,-5.84422216200635));
#4122=CARTESIAN_POINT('Ctrl Pts',(-12.4302293937643,1.,-5.84422216200635));
#4123=CARTESIAN_POINT('Origin',(-12.4302293937643,0.,0.));
#4124=CARTESIAN_POINT('',(-13.4302293937643,-3.9801020972289E-16,-4.5));
#4125=CARTESIAN_POINT('Origin',(-12.4302293937643,-2.75545529808154E-16,
-4.5));
#4126=CARTESIAN_POINT('',(-13.4302293937643,1.22464679914735E-16,-7.49879891330929E-33));
#4127=CARTESIAN_POINT('Origin',(-12.4302293937643,8.26636589424463E-16,
4.5));
#4128=CARTESIAN_POINT('Origin',(-12.4302293937643,4.5,-5.51091059616309E-16));
#4129=CARTESIAN_POINT('Origin',(-12.4302293937643,-2.75545529808154E-16,
-4.5));
#4130=CARTESIAN_POINT('Ctrl Pts',(-12.4302293937643,-6.08893299837349,-1.29488563599616));
#4131=CARTESIAN_POINT('Ctrl Pts',(-12.5942556094579,-6.08893299096372,-1.29488562495703));
#4132=CARTESIAN_POINT('Ctrl Pts',(-12.9435199759374,-6.10362004692185,-1.22941547699904));
#4133=CARTESIAN_POINT('Ctrl Pts',(-13.2353124874664,-6.14033341252253,-1.03140005307915));
#4134=CARTESIAN_POINT('Ctrl Pts',(-13.4654077531044,-6.17434194926064,-0.80247914861247));
#4135=CARTESIAN_POINT('Ctrl Pts',(-13.6642012577212,-6.21070412871452,-0.511738560164233));
#4136=CARTESIAN_POINT('Ctrl Pts',(-13.7305928319399,-6.2253945953946,-0.163672629624612));
#4137=CARTESIAN_POINT('Ctrl Pts',(-13.7305735234977,-6.22536971833509,0.163413942637349));
#4138=CARTESIAN_POINT('Ctrl Pts',(-13.6641961660918,-6.21065684408847,0.511524716651758));
#4139=CARTESIAN_POINT('Ctrl Pts',(-13.465346435092,-6.17428139683409,0.802173448767081));
#4140=CARTESIAN_POINT('Ctrl Pts',(-13.2353970954988,-6.14016146593015,1.0312922208101));
#4141=CARTESIAN_POINT('Ctrl Pts',(-13.0896053944545,-6.12196313951551,1.13039533120231));
#4142=CARTESIAN_POINT('Ctrl Pts',(-12.7690837661183,-6.09606085401061,1.2622143813522));
#4143=CARTESIAN_POINT('Ctrl Pts',(-12.5943834161953,-6.08887828006945,1.2946897058071));
#4144=CARTESIAN_POINT('Ctrl Pts',(-12.2661932789077,-6.08887357909258,1.29460046621699));
#4145=CARTESIAN_POINT('Ctrl Pts',(-12.0914931498336,-6.09604795264992,1.26198004011685));
#4146=CARTESIAN_POINT('Ctrl Pts',(-11.7709848415179,-6.12194030356741,1.12995676459186));
#4147=CARTESIAN_POINT('Ctrl Pts',(-11.6251708828575,-6.14012997800531,1.03077281364708));
#4148=CARTESIAN_POINT('Ctrl Pts',(-11.4025000109833,-6.17317174739286,0.808380882336614));
#4149=CARTESIAN_POINT('Ctrl Pts',(-11.2517604169044,-6.20030388726032,0.59559414446078));
#4150=CARTESIAN_POINT('Ctrl Pts',(-11.1346832359419,-6.22414177319952,0.217454422107557));
#4151=CARTESIAN_POINT('Ctrl Pts',(-11.1179113891857,-6.2277097295171,-0.121675282907419));
#4152=CARTESIAN_POINT('Ctrl Pts',(-11.1792551432517,-6.2148909110589,-0.376842015671391));
#4153=CARTESIAN_POINT('Ctrl Pts',(-11.2952430555643,-6.19246471770926,-0.656705157785398));
#4154=CARTESIAN_POINT('Ctrl Pts',(-11.3950443526158,-6.17434641001338,-0.801855766228741));
#4155=CARTESIAN_POINT('Ctrl Pts',(-11.6251511260733,-6.14020362776066,-1.03103200836982));
#4156=CARTESIAN_POINT('Ctrl Pts',(-11.7709033259227,-6.122014163478,-1.13030300160637));
#4157=CARTESIAN_POINT('Ctrl Pts',(-12.0914373624932,-6.09611196893258,-1.26225531127416));
#4158=CARTESIAN_POINT('Ctrl Pts',(-12.2662031836223,-6.08893299149969,-1.29488564095978));
#4159=CARTESIAN_POINT('Ctrl Pts',(-12.4302293937643,-6.08893299837349,-1.29488563599616));
#4160=CARTESIAN_POINT('Ctrl Pts',(-12.4302293937643,-6.00730670135932,-1.19652291995803));
#4161=CARTESIAN_POINT('Ctrl Pts',(-12.5835416075593,-6.00733185292099,-1.19656039090436));
#4162=CARTESIAN_POINT('Ctrl Pts',(-12.9099992478929,-6.02016943668172,-1.13400457500984));
#4163=CARTESIAN_POINT('Ctrl Pts',(-13.179481120053,-6.05208117737328,-0.947735263929781));
#4164=CARTESIAN_POINT('Ctrl Pts',(-13.3905508253865,-6.08150297834998,-0.734658226364409));
#4165=CARTESIAN_POINT('Ctrl Pts',(-13.5709920959587,-6.11274177608899,-0.466042577449154));
#4166=CARTESIAN_POINT('Ctrl Pts',(-13.6304639246011,-6.12529782064175,-0.149051739413726));
#4167=CARTESIAN_POINT('Ctrl Pts',(-13.6304533897943,-6.12527260806574,0.148787647638987));
#4168=CARTESIAN_POINT('Ctrl Pts',(-13.5709720447989,-6.11269507902186,0.465848644629128));
#4169=CARTESIAN_POINT('Ctrl Pts',(-13.3905041431794,-6.08144180450652,0.734326683901586));
#4170=CARTESIAN_POINT('Ctrl Pts',(-13.1795428364226,-6.05191130345156,0.947674493001592));
#4171=CARTESIAN_POINT('Ctrl Pts',(-13.0449586384788,-6.03611037539515,1.04079617562098));
#4172=CARTESIAN_POINT('Ctrl Pts',(-12.7469388659841,-6.01354168438538,1.16540284340237));
#4173=CARTESIAN_POINT('Ctrl Pts',(-12.5836962315238,-6.00726039156444,1.19631326107954));
#4174=CARTESIAN_POINT('Ctrl Pts',(-12.2768814243267,-6.00725251877471,1.19624527202557));
#4175=CARTESIAN_POINT('Ctrl Pts',(-12.1136335971426,-6.01353340392645,1.16513750020312));
#4176=CARTESIAN_POINT('Ctrl Pts',(-11.8156395078111,-6.03608069520521,1.04040354702773));
#4177=CARTESIAN_POINT('Ctrl Pts',(-11.6810080385117,-6.0518936089174,0.947061071249189));
#4178=CARTESIAN_POINT('Ctrl Pts',(-11.476775432527,-6.0804537040016,0.740195388112021));
#4179=CARTESIAN_POINT('Ctrl Pts',(-11.3397927474364,-6.1038110687889,0.543436243686021));
#4180=CARTESIAN_POINT('Ctrl Pts',(-11.2343328423298,-6.12419591144059,0.197848988748778));
#4181=CARTESIAN_POINT('Ctrl Pts',(-11.2192240525651,-6.12725896708914,-0.110526507186422));
#4182=CARTESIAN_POINT('Ctrl Pts',(-11.2744078114987,-6.11629204566253,-0.343438032428988));
#4183=CARTESIAN_POINT('Ctrl Pts',(-11.3792086385588,-6.09709227633881,-0.599872706676036));
#4184=CARTESIAN_POINT('Ctrl Pts',(-11.4699522513166,-6.08147950050026,-0.734057964386069));
#4185=CARTESIAN_POINT('Ctrl Pts',(-11.6809647607171,-6.05196881986237,-0.947385415737105));
#4186=CARTESIAN_POINT('Ctrl Pts',(-11.8155701530245,-6.03615792504545,-1.04071590511793));
#4187=CARTESIAN_POINT('Ctrl Pts',(-12.1135691209239,-6.01358992981694,-1.1654384548815));
#4188=CARTESIAN_POINT('Ctrl Pts',(-12.2768983357228,-6.00733003360885,-1.19650607159156));
#4189=CARTESIAN_POINT('Ctrl Pts',(-12.4302293937643,-6.00730670135932,-1.19652291995803));
#4190=CARTESIAN_POINT('Ctrl Pts',(-12.4302293937643,-5.92568040434515,-1.09816020391989));
#4191=CARTESIAN_POINT('Ctrl Pts',(-12.5728617871465,-5.92565520838872,-1.09812266683399));
#4192=CARTESIAN_POINT('Ctrl Pts',(-12.8764307452579,-5.93669281540111,-1.03868333620408));
#4193=CARTESIAN_POINT('Ctrl Pts',(-13.1237066796822,-5.96381552620845,-0.863916643031107));
#4194=CARTESIAN_POINT('Ctrl Pts',(-13.3156785658162,-5.98860458124536,-0.666696003113148));
#4195=CARTESIAN_POINT('Ctrl Pts',(-13.4779257102115,-6.01480861265757,-0.420423936232896));
#4196=CARTESIAN_POINT('Ctrl Pts',(-13.5302115977681,-6.0251142009875,-0.134359645298094));
#4197=CARTESIAN_POINT('Ctrl Pts',(-13.5301694517177,-6.02509693896035,0.134284106327718));
#4198=CARTESIAN_POINT('Ctrl Pts',(-13.4779135143473,-6.01477545935064,0.420354149772739));
#4199=CARTESIAN_POINT('Ctrl Pts',(-13.3155662884545,-5.98856196814462,0.666614474975836));
#4200=CARTESIAN_POINT('Ctrl Pts',(-13.1237490229197,-5.96369791624148,0.863960278040423));
#4201=CARTESIAN_POINT('Ctrl Pts',(-13.0002570596326,-5.95026526779515,0.951291302906749));
#4202=CARTESIAN_POINT('Ctrl Pts',(-12.7248192878539,-5.93103075476377,1.06853916455731));
#4203=CARTESIAN_POINT('Ctrl Pts',(-12.5729580288434,-5.92565006141073,1.09800243214524));
#4204=CARTESIAN_POINT('Ctrl Pts',(-12.287577286871,-5.92565044560247,1.09790991870327));
#4205=CARTESIAN_POINT('Ctrl Pts',(-12.1357205964749,-5.9310187003764,1.06838177460848));
#4206=CARTESIAN_POINT('Ctrl Pts',(-11.8602821295538,-5.9502584447237,0.950895885550572));
#4207=CARTESIAN_POINT('Ctrl Pts',(-11.736788079086,-5.96366715170961,0.863629609851932));
#4208=CARTESIAN_POINT('Ctrl Pts',(-11.5510151221346,-5.98777821987636,0.67188359125213));
#4209=CARTESIAN_POINT('Ctrl Pts',(-11.427751170242,-6.00731764764785,0.491487465397297));
#4210=CARTESIAN_POINT('Ctrl Pts',(-11.3339016795611,-6.02427343221154,0.178379449022163));
#4211=CARTESIAN_POINT('Ctrl Pts',(-11.3206116198576,-6.02677974461079,-0.0997509032157466));
#4212=CARTESIAN_POINT('Ctrl Pts',(-11.3695095553554,-6.01770990863714,-0.310016341778994));
#4213=CARTESIAN_POINT('Ctrl Pts',(-11.463356556165,-6.00165061145685,-0.543287387943066));
#4214=CARTESIAN_POINT('Ctrl Pts',(-11.5448540553375,-5.98861113270541,-0.666319219911386));
#4215=CARTESIAN_POINT('Ctrl Pts',(-11.7368736448428,-5.96369271832399,-0.86381896190319));
#4216=CARTESIAN_POINT('Ctrl Pts',(-11.8602625947015,-5.95028583599656,-0.951226144039803));
#4217=CARTESIAN_POINT('Ctrl Pts',(-12.1357218721558,-5.93105211422019,-1.06859726081973));
#4218=CARTESIAN_POINT('Ctrl Pts',(-12.2876158778903,-5.92565703091211,-1.09817708202523));
#4219=CARTESIAN_POINT('Ctrl Pts',(-12.4302293937643,-5.92568040434515,-1.09816020391989));
#4220=CARTESIAN_POINT('Ctrl Pts',(-12.4302293937643,-5.84405410733098,-0.999797487881759));
#4221=CARTESIAN_POINT('Ctrl Pts',(-12.5621477450218,-5.84405415920521,-0.999797565164297));
#4222=CARTESIAN_POINT('Ctrl Pts',(-12.8429100734364,-5.85324223577186,-0.943272328695468));
#4223=CARTESIAN_POINT('Ctrl Pts',(-13.0678752452747,-5.87556330684772,-0.780252034917407));
#4224=CARTESIAN_POINT('Ctrl Pts',(-13.2408216561416,-5.89576568026994,-0.598875247154049));
#4225=CARTESIAN_POINT('Ctrl Pts',(-13.3847163804241,-5.91684622568096,-0.374727862499088));
#4226=CARTESIAN_POINT('Ctrl Pts',(-13.4300828356746,-5.9250175284374,-0.119738838882957));
#4227=CARTESIAN_POINT('Ctrl Pts',(-13.4300495107861,-5.92499992114235,0.119657666867655));
#4228=CARTESIAN_POINT('Ctrl Pts',(-13.3846891981801,-5.91681364468555,0.374677864062464));
#4229=CARTESIAN_POINT('Ctrl Pts',(-13.2407241090043,-5.89572242317792,0.598767551759252));
#4230=CARTESIAN_POINT('Ctrl Pts',(-13.0678946927086,-5.87544771048421,0.780342663782052));
#4231=CARTESIAN_POINT('Ctrl Pts',(-12.9556103681747,-5.86441249466429,0.861692036369364));
#4232=CARTESIAN_POINT('Ctrl Pts',(-12.7026743579198,-5.84851157544137,0.97172768796908));
#4233=CARTESIAN_POINT('Ctrl Pts',(-12.562270904212,-5.84403216401073,0.999625910198263));
#4234=CARTESIAN_POINT('Ctrl Pts',(-12.2982654232083,-5.84402936293972,0.999554701162274));
#4235=CARTESIAN_POINT('Ctrl Pts',(-12.1578611066837,-5.84850415183514,0.971539132528016));
#4236=CARTESIAN_POINT('Ctrl Pts',(-11.9049368100215,-5.86439879239718,0.861342614374135));
#4237=CARTESIAN_POINT('Ctrl Pts',(-11.7926253019556,-5.87543077095699,0.779917537607569));
#4238=CARTESIAN_POINT('Ctrl Pts',(-11.625290585729,-5.89506012639956,0.603698245665789));
#4239=CARTESIAN_POINT('Ctrl Pts',(-11.5157835877516,-5.91082482988569,0.439329318518403));
#4240=CARTESIAN_POINT('Ctrl Pts',(-11.4335513810015,-5.92432754293507,0.158773855738042));
#4241=CARTESIAN_POINT('Ctrl Pts',(-11.421924195087,-5.92632901567582,-0.0886016883305396));
#4242=CARTESIAN_POINT('Ctrl Pts',(-11.4646622835325,-5.91911102355411,-0.276612379375412));
#4243=CARTESIAN_POINT('Ctrl Pts',(-11.5473219245805,-5.90627825155154,-0.486454645997929));
#4244=CARTESIAN_POINT('Ctrl Pts',(-11.6197619612107,-5.89574422490846,-0.59852134856752));
#4245=CARTESIAN_POINT('Ctrl Pts',(-11.792687167393,-5.87545795902179,-0.78017227495977));
#4246=CARTESIAN_POINT('Ctrl Pts',(-11.904929391659,-5.86442961621768,-0.861638933002959));
#4247=CARTESIAN_POINT('Ctrl Pts',(-12.1578536058814,-5.84853009367097,-0.971780433068657));
#4248=CARTESIAN_POINT('Ctrl Pts',(-12.2983110036412,-5.84405415545294,-0.999797453132582));
#4249=CARTESIAN_POINT('Ctrl Pts',(-12.4302293937643,-5.84405410733098,-0.999797487881759));
#4250=CARTESIAN_POINT('',(-12.4302293937643,-5.84422216200635,-1.));
#4251=CARTESIAN_POINT('',(-12.4302293937643,-6.08890895085005,-1.29485665783831));
#4252=CARTESIAN_POINT('',(-13.4302293937643,-5.9251719038059,1.0785270517389E-16));
#4253=CARTESIAN_POINT('Ctrl Pts',(-12.4302293937643,-5.84422216200635,-1.));
#4254=CARTESIAN_POINT('Ctrl Pts',(-12.4944982458915,-5.84422216200635,-1.));
#4255=CARTESIAN_POINT('Ctrl Pts',(-12.5587518483679,-5.84562231156004,-0.993793077287905));
#4256=CARTESIAN_POINT('Ctrl Pts',(-12.6840917070905,-5.84953577508847,-0.969312352511264));
#4257=CARTESIAN_POINT('Ctrl Pts',(-12.7449916575148,-5.85204625647294,-0.951276694198755));
#4258=CARTESIAN_POINT('Ctrl Pts',(-12.864337458649,-5.85877465283481,-0.903230714929781));
#4259=CARTESIAN_POINT('Ctrl Pts',(-12.9223384459871,-5.8632652060475,-0.872966477219125));
#4260=CARTESIAN_POINT('Ctrl Pts',(-13.0310521006909,-5.87276344316928,-0.801996314727874));
#4261=CARTESIAN_POINT('Ctrl Pts',(-13.0816795448316,-5.87769727434892,-0.761443393429155));
#4262=CARTESIAN_POINT('Ctrl Pts',(-13.1735637062492,-5.88774709930129,-0.671936344908102));
#4263=CARTESIAN_POINT('Ctrl Pts',(-13.2147234026552,-5.89313164041396,-0.623382463895755));
#4264=CARTESIAN_POINT('Ctrl Pts',(-13.2878087312711,-5.90320437241943,-0.518368774693091));
#4265=CARTESIAN_POINT('Ctrl Pts',(-13.3194196283319,-5.90778220806811,-0.462062726244169));
#4266=CARTESIAN_POINT('Ctrl Pts',(-13.3714221289722,-5.91556605482255,-0.343975848624026));
#4267=CARTESIAN_POINT('Ctrl Pts',(-13.3917043040785,-5.91892406306771,-0.282400092474657));
#4268=CARTESIAN_POINT('Ctrl Pts',(-13.420000040749,-5.92359300815781,-0.156508651779502));
#4269=CARTESIAN_POINT('Ctrl Pts',(-13.4280159105558,-5.92484933356782,-0.0925661452570473));
#4270=CARTESIAN_POINT('Ctrl Pts',(-13.4300968211925,-5.92515214681615,-0.0188017619570889));
#4271=CARTESIAN_POINT('Ctrl Pts',(-13.4302293937643,-5.9251709568609,-0.00940098878205599));
#4272=CARTESIAN_POINT('Ctrl Pts',(-13.4302293937643,-5.9251719038059,-4.20390922051782E-16));
#4273=CARTESIAN_POINT('Ctrl Pts',(-13.4302293937643,-5.9251719038059,-4.20390922051782E-16));
#4274=CARTESIAN_POINT('Ctrl Pts',(-13.4302293937643,-5.92517721135784,0.0526917995608284));
#4275=CARTESIAN_POINT('Ctrl Pts',(-13.4260601515651,-5.92458148056859,0.105390376886493));
#4276=CARTESIAN_POINT('Ctrl Pts',(-13.4077283650324,-5.92160517649706,0.220319257946971));
#4277=CARTESIAN_POINT('Ctrl Pts',(-13.3917600419347,-5.91889366817302,0.281942156475162));
#4278=CARTESIAN_POINT('Ctrl Pts',(-13.3480477817509,-5.91202032426913,0.402198254109568));
#4279=CARTESIAN_POINT('Ctrl Pts',(-13.3202407961492,-5.90795462801506,0.460471360524695));
#4280=CARTESIAN_POINT('Ctrl Pts',(-13.2535116311086,-5.89846585980263,0.57133537793989));
#4281=CARTESIAN_POINT('Ctrl Pts',(-13.2146990232233,-5.89303091664152,0.623545922817736));
#4282=CARTESIAN_POINT('Ctrl Pts',(-13.1291961220027,-5.8825630261041,0.717879440332942));
#4283=CARTESIAN_POINT('Ctrl Pts',(-13.0830058863189,-5.87774668100827,0.76012306424411));
#4284=CARTESIAN_POINT('Ctrl Pts',(-12.9826770102536,-5.86824548138472,0.83594569086839));
#4285=CARTESIAN_POINT('Ctrl Pts',(-12.9286733506225,-5.86357871145779,0.869229122032554));
#4286=CARTESIAN_POINT('Ctrl Pts',(-12.814646447115,-5.85546947246655,0.925361834437775));
#4287=CARTESIAN_POINT('Ctrl Pts',(-12.7550536475759,-5.85234789442664,0.947920256643328));
#4288=CARTESIAN_POINT('Ctrl Pts',(-12.6077286786872,-5.84664782631375,0.988134290189823));
#4289=CARTESIAN_POINT('Ctrl Pts',(-12.5190391995663,-5.84434890472074,0.999996557140233));
#4290=CARTESIAN_POINT('Ctrl Pts',(-12.3414508870207,-5.84439252370977,1.00000344312345));
#4291=CARTESIAN_POINT('Ctrl Pts',(-12.2527245841438,-5.84675093906306,0.988135859292573));
#4292=CARTESIAN_POINT('Ctrl Pts',(-12.1053731550729,-5.85253966996574,0.947909320920726));
#4293=CARTESIAN_POINT('Ctrl Pts',(-12.0457787622019,-5.85569317128686,0.925347745846651));
#4294=CARTESIAN_POINT('Ctrl Pts',(-11.9317032574863,-5.86385480068626,0.869186241970665));
#4295=CARTESIAN_POINT('Ctrl Pts',(-11.8776535063375,-5.86854502214797,0.835865276146026));
#4296=CARTESIAN_POINT('Ctrl Pts',(-11.7771843657185,-5.87810913986364,0.759903727134754));
#4297=CARTESIAN_POINT('Ctrl Pts',(-11.7309014155548,-5.88301655964537,0.717535821849503));
#4298=CARTESIAN_POINT('Ctrl Pts',(-11.6446884611433,-5.89355171795038,0.622305619278858));
#4299=CARTESIAN_POINT('Ctrl Pts',(-11.6053836802498,-5.89886076131314,0.56919270515609));
#4300=CARTESIAN_POINT('Ctrl Pts',(-11.5549487679018,-5.90590573411597,0.484702051427652));
#4301=CARTESIAN_POINT('Ctrl Pts',(-11.5396848313392,-5.90809410537879,0.456052361783949));
#4302=CARTESIAN_POINT('Ctrl Pts',(-11.4984673381252,-5.91423227905847,0.368691539381281));
#4303=CARTESIAN_POINT('Ctrl Pts',(-11.4766739314384,-5.91795523502758,0.308013717888738));
#4304=CARTESIAN_POINT('Ctrl Pts',(-11.445711632252,-5.92296069604394,0.185827526072649));
#4305=CARTESIAN_POINT('Ctrl Pts',(-11.436138601018,-5.9242390513156,0.124800058789788));
#4306=CARTESIAN_POINT('Ctrl Pts',(-11.428157368614,-5.92535267058096,-0.000936975829386351));
#4307=CARTESIAN_POINT('Ctrl Pts',(-11.4302996049242,-5.92520408286643,-0.0656208398590233));
#4308=CARTESIAN_POINT('Ctrl Pts',(-11.447092733453,-5.92251839001045,-0.19408607762655));
#4309=CARTESIAN_POINT('Ctrl Pts',(-11.4617712884571,-5.91996522088789,-0.25749448426409));
#4310=CARTESIAN_POINT('Ctrl Pts',(-11.5032325236537,-5.91324612004577,-0.380667291322442));
#4311=CARTESIAN_POINT('Ctrl Pts',(-11.5299666236449,-5.90927771739317,-0.44018443126589));
#4312=CARTESIAN_POINT('Ctrl Pts',(-11.5783475393985,-5.90247649310005,-0.524730963460824));
#4313=CARTESIAN_POINT('Ctrl Pts',(-11.595748617846,-5.90006780571956,-0.551983456838474));
#4314=CARTESIAN_POINT('Ctrl Pts',(-11.651223457358,-5.89258038162579,-0.630234975445558));
#4315=CARTESIAN_POINT('Ctrl Pts',(-11.6928573009781,-5.88719076659233,-0.678478398391647));
#4316=CARTESIAN_POINT('Ctrl Pts',(-11.785608298049,-5.87706819763353,-0.767238038743982));
#4317=CARTESIAN_POINT('Ctrl Pts',(-11.8366404907297,-5.87210453132499,-0.807369546161976));
#4318=CARTESIAN_POINT('Ctrl Pts',(-11.946000874798,-5.86260028948649,-0.877358832991084));
#4319=CARTESIAN_POINT('Ctrl Pts',(-12.0042344687816,-5.85810609494132,-0.907081501893602));
#4320=CARTESIAN_POINT('Ctrl Pts',(-12.1237240476056,-5.8514570651785,-0.953952809540106));
#4321=CARTESIAN_POINT('Ctrl Pts',(-12.1845405832366,-5.849045354789,-0.971400470233401));
#4322=CARTESIAN_POINT('Ctrl Pts',(-12.307144058756,-5.84544554810484,-0.994307498142081));
#4323=CARTESIAN_POINT('Ctrl Pts',(-12.3686784358337,-5.84422216200635,-1.));
#4324=CARTESIAN_POINT('Ctrl Pts',(-12.4302293937643,-5.84422216200635,-1.));
#4325=CARTESIAN_POINT('Origin',(-12.4302293937643,0.,0.));
#4326=CARTESIAN_POINT('',(-13.4302293937643,-4.5,1.22464679914735E-16));
#4327=CARTESIAN_POINT('Origin',(-12.4302293937643,-4.5,0.));
#4328=CARTESIAN_POINT('',(-13.4302293937643,0.,-1.22464679914735E-16));
#4329=CARTESIAN_POINT('Origin',(-12.4302293937643,-4.5,0.));
#4330=CARTESIAN_POINT('Origin',(-14.3242463976144,0.,-5.96248981933611));
#4331=CARTESIAN_POINT('',(-14.3242463976144,-7.30194407219864E-16,5.96248981933611));
#4332=CARTESIAN_POINT('Origin',(-14.3242463976144,0.,0.));
#4333=CARTESIAN_POINT('',(-14.3242463976144,-4.4393205576042E-16,3.62498032958974));
#4334=CARTESIAN_POINT('Origin',(-14.3242463976144,0.,0.));
#4335=CARTESIAN_POINT('Origin',(-14.2019363570046,0.,0.));
#4336=CARTESIAN_POINT('',(-14.2019363570046,-7.46272655961369E-16,6.09377868362497));
#4337=CARTESIAN_POINT('Origin',(-10.6585224305239,0.,0.));
#4338=CARTESIAN_POINT('',(-10.5362123899142,-7.30194407219864E-16,5.96248981933611));
#4339=CARTESIAN_POINT('',(-10.6585224305239,7.46272655961369E-16,6.09377868362497));
#4340=CARTESIAN_POINT('Origin',(-10.5362123899142,0.,0.));
#4341=CARTESIAN_POINT('Origin',(-10.5362123899142,0.,-3.62498032958974));
#4342=CARTESIAN_POINT('',(-10.5362123899142,-4.4393205576042E-16,3.62498032958974));
#4343=CARTESIAN_POINT('Origin',(-10.5362123899142,0.,0.));
#4344=CARTESIAN_POINT('Origin',(-10.6678019790643,0.,0.));
#4345=CARTESIAN_POINT('',(-10.7993915682143,-3.88369225985197E-16,3.17127539348974));
#4346=CARTESIAN_POINT('Origin',(-10.7993915682143,0.,0.));
#4347=CARTESIAN_POINT('',(-10.6678019790643,-4.16150640872808E-16,3.39812786153974));
#4348=CARTESIAN_POINT('Origin',(-12.4302293937643,0.,0.));
#4349=CARTESIAN_POINT('',(-14.0610672193142,-3.88369225985197E-16,3.17127539348974));
#4350=CARTESIAN_POINT('Origin',(-14.0610672193142,0.,0.));
#4351=CARTESIAN_POINT('',(-12.4302293937643,-3.88369225985197E-16,3.17127539348974));
#4352=CARTESIAN_POINT('Origin',(-14.1926568084643,0.,0.));
#4353=CARTESIAN_POINT('',(-14.1926568084643,4.16150640872808E-16,3.39812786153974));
#4354=CARTESIAN_POINT('',(0.,0.,0.));
#4355=CARTESIAN_POINT('Origin',(-32.0305529756126,-0.749999999999998,0.));
#4356=CARTESIAN_POINT('',(-26.9411105316953,-0.749999999999998,-2.57875622086151));
#4357=CARTESIAN_POINT('',(-24.9598233877886,-0.749999999999997,-2.57875622086151));
#4358=CARTESIAN_POINT('',(-25.7922242605427,-0.749999999999997,-2.57875622086151));
#4359=CARTESIAN_POINT('',(-26.9411105316953,-0.749999999999998,-1.83684484821367));
#4360=CARTESIAN_POINT('',(-26.9411105316953,-0.749999999999998,-1.34280337788449));
#4361=CARTESIAN_POINT('',(-24.9598233877886,-0.749999999999997,-1.83684484821367));
#4362=CARTESIAN_POINT('',(-21.6665165759647,-0.749999999999997,-1.83684484821367));
#4363=CARTESIAN_POINT('',(-24.9598233877886,-0.749999999999997,0.));
#4364=CARTESIAN_POINT('Origin',(-32.0305529756126,-0.749999999999998,0.));
#4365=CARTESIAN_POINT('',(-24.9598233877886,-0.749999999999997,2.57875622086151));
#4366=CARTESIAN_POINT('',(-26.9411105316953,-0.749999999999998,2.57875622086151));
#4367=CARTESIAN_POINT('',(-25.7922242605427,-0.749999999999997,2.57875622086151));
#4368=CARTESIAN_POINT('',(-24.9598233877886,-0.749999999999997,1.83684484821367));
#4369=CARTESIAN_POINT('',(-24.9598233877886,-0.749999999999997,0.));
#4370=CARTESIAN_POINT('',(-26.9411105316953,-0.749999999999998,1.83684484821367));
#4371=CARTESIAN_POINT('',(-21.6665165759647,-0.749999999999997,1.83684484821367));
#4372=CARTESIAN_POINT('',(-26.9411105316953,-0.749999999999998,-1.34280337788449));
#4373=CARTESIAN_POINT('Origin',(-24.9598233877886,-0.0500000000000033,0.));
#4374=CARTESIAN_POINT('',(-24.6433379893901,-0.674369275830021,-2.59955952546743));
#4375=CARTESIAN_POINT('Ctrl Pts',(-24.9598233877886,-0.749999999999997,
-2.57875622086151));
#4376=CARTESIAN_POINT('Ctrl Pts',(-24.8714588989999,-0.749999999999997,
-2.57875622086151));
#4377=CARTESIAN_POINT('Ctrl Pts',(-24.7775423290656,-0.732251654012554,
-2.58411714720213));
#4378=CARTESIAN_POINT('Ctrl Pts',(-24.6751102588048,-0.689726977700767,
-2.59553646483285));
#4379=CARTESIAN_POINT('Ctrl Pts',(-24.6590554485685,-0.682336269919017,
-2.59749275377718));
#4380=CARTESIAN_POINT('Ctrl Pts',(-24.6433379893901,-0.674369275830042,
-2.59955952546742));
#4381=CARTESIAN_POINT('',(-24.2598233877886,-0.0499999999999985,-1.9834311171324));
#4382=CARTESIAN_POINT('Ctrl Pts',(-24.2598233877886,-0.0500000000000034,
-1.9834311171324));
#4383=CARTESIAN_POINT('Ctrl Pts',(-24.2598233877886,-0.139024680847254,
-1.98118690809287));
#4384=CARTESIAN_POINT('Ctrl Pts',(-24.2778228093247,-0.233283857786286,
-1.97223255425957));
#4385=CARTESIAN_POINT('Ctrl Pts',(-24.349705656948,-0.405631974937099,-1.94411555901275));
#4386=CARTESIAN_POINT('Ctrl Pts',(-24.4035428766891,-0.483787439248121,
-1.92524336790881));
#4387=CARTESIAN_POINT('Ctrl Pts',(-24.5269368573565,-0.606943918256759,
-1.89002872240561));
#4388=CARTESIAN_POINT('Ctrl Pts',(-24.6049717534738,-0.660537412507157,
-1.87126930464578));
#4389=CARTESIAN_POINT('Ctrl Pts',(-24.7769694082335,-0.732084988974823,
-1.8444538864071));
#4390=CARTESIAN_POINT('Ctrl Pts',(-24.8710178004329,-0.749999999999997,
-1.83684484821367));
#4391=CARTESIAN_POINT('Ctrl Pts',(-24.9598233877886,-0.749999999999997,
-1.83684484821367));
#4392=CARTESIAN_POINT('',(-24.2598233877886,-0.0499999999999985,-2.72441956476416));
#4393=CARTESIAN_POINT('',(-24.2598233877886,-0.0499999999999985,0.));
#4394=CARTESIAN_POINT('Ctrl Pts',(-24.6433379893901,-0.674369275830043,
-2.59955952546742));
#4395=CARTESIAN_POINT('Ctrl Pts',(-24.5848581377007,-0.64472653094067,-2.60724934991992));
#4396=CARTESIAN_POINT('Ctrl Pts',(-24.531196418248,-0.607203802215661,-2.61926288147073));
#4397=CARTESIAN_POINT('Ctrl Pts',(-24.4188018998553,-0.502917996238797,
-2.65129970036023));
#4398=CARTESIAN_POINT('Ctrl Pts',(-24.3656895097955,-0.430698662203228,
-2.67244287095924));
#4399=CARTESIAN_POINT('Ctrl Pts',(-24.2967339716088,-0.285490706378351,
-2.70312656992203));
#4400=CARTESIAN_POINT('Ctrl Pts',(-24.2758927310872,-0.215972246591974,
-2.71398152997755));
#4401=CARTESIAN_POINT('Ctrl Pts',(-24.2619469726382,-0.112808220815181,
-2.72227581593582));
#4402=CARTESIAN_POINT('Ctrl Pts',(-24.2598338408088,-0.081573716422347,
-2.72383525661314));
#4403=CARTESIAN_POINT('Ctrl Pts',(-24.2598234264347,-0.0502326037857873,
-2.72441527796272));
#4404=CARTESIAN_POINT('Ctrl Pts',(-24.2598234006703,-0.0501550682186355,
-2.72441671289213));
#4405=CARTESIAN_POINT('Ctrl Pts',(-24.2598233877886,-0.0500775336225404,
-2.7244181418258));
#4406=CARTESIAN_POINT('Ctrl Pts',(-24.2598233877886,-0.0499999999999986,
-2.72441956476417));
#4407=CARTESIAN_POINT('Origin',(-24.2598233877886,-0.0499999999999985,0.));
#4408=CARTESIAN_POINT('',(-24.2598233877886,0.0500000000000051,-2.72441956476416));
#4409=CARTESIAN_POINT('Origin',(-24.2598233877886,0.,0.));
#4410=CARTESIAN_POINT('',(-24.2598233877886,0.0500000000000051,-1.9834311171324));
#4411=CARTESIAN_POINT('Origin',(-24.2598233877886,0.,0.));
#4412=CARTESIAN_POINT('',(-24.2598233877886,0.0500000000000051,0.));
#4413=CARTESIAN_POINT('Origin',(-24.9598233877886,0.750000000000003,0.));
#4414=CARTESIAN_POINT('',(-24.9598233877886,0.750000000000003,-2.57875622086151));
#4415=CARTESIAN_POINT('',(-26.9411105316953,0.750000000000003,-2.57875622086151));
#4416=CARTESIAN_POINT('',(-25.7922242605427,0.750000000000003,-2.57875622086151));
#4417=CARTESIAN_POINT('',(-24.9598233877886,0.750000000000003,-1.83684484821366));
#4418=CARTESIAN_POINT('',(-24.9598233877886,0.750000000000003,0.));
#4419=CARTESIAN_POINT('',(-26.9411105316953,0.750000000000003,-1.83684484821366));
#4420=CARTESIAN_POINT('',(-21.6665165759647,0.750000000000004,-1.83684484821366));
#4421=CARTESIAN_POINT('',(-26.9411105316953,0.750000000000003,-1.34280337788449));
#4422=CARTESIAN_POINT('Origin',(-24.9598233877886,0.050000000000005,0.));
#4423=CARTESIAN_POINT('',(-24.6433379893901,0.674369275830023,-2.59955952546743));
#4424=CARTESIAN_POINT('Ctrl Pts',(-24.2598233877886,0.0500000000000053,
-2.72441956476417));
#4425=CARTESIAN_POINT('Ctrl Pts',(-24.2598233877886,0.0500775341306451,
-2.72441814181648));
#4426=CARTESIAN_POINT('Ctrl Pts',(-24.2598234006705,0.0501550687267315,
-2.72441671288273));
#4427=CARTESIAN_POINT('Ctrl Pts',(-24.2598234264347,0.050232603785789,-2.72441527796272));
#4428=CARTESIAN_POINT('Ctrl Pts',(-24.2598455995816,0.116960674997039,-2.72318035990581));
#4429=CARTESIAN_POINT('Ctrl Pts',(-24.2693721788655,0.182817524037613,-2.71744107277057));
#4430=CARTESIAN_POINT('Ctrl Pts',(-24.3111665384102,0.325934269006048,-2.69640279204955));
#4431=CARTESIAN_POINT('Ctrl Pts',(-24.3482258638932,0.400187099831499,-2.67924676947619));
#4432=CARTESIAN_POINT('Ctrl Pts',(-24.451725722152,0.540287158645911,-2.64091034959975));
#4433=CARTESIAN_POINT('Ctrl Pts',(-24.5211658067261,0.603472684928343,-2.61969621846221));
#4434=CARTESIAN_POINT('Ctrl Pts',(-24.615213593946,0.659505977432703,-2.60354842317404));
#4435=CARTESIAN_POINT('Ctrl Pts',(-24.6291544833972,0.667179824461095,-2.60142458955455));
#4436=CARTESIAN_POINT('Ctrl Pts',(-24.6433379893901,0.674369275830048,-2.59955952546742));
#4437=CARTESIAN_POINT('Ctrl Pts',(-24.9598233877886,0.750000000000003,-1.83684484821366));
#4438=CARTESIAN_POINT('Ctrl Pts',(-24.8710178004329,0.750000000000002,-1.83684484821366));
#4439=CARTESIAN_POINT('Ctrl Pts',(-24.7769694082335,0.732084988974827,-1.84445388640709));
#4440=CARTESIAN_POINT('Ctrl Pts',(-24.6049717534738,0.660537412507157,-1.87126930464578));
#4441=CARTESIAN_POINT('Ctrl Pts',(-24.5269368573564,0.606943918256764,-1.89002872240561));
#4442=CARTESIAN_POINT('Ctrl Pts',(-24.4035428766891,0.483787439248125,-1.92524336790881));
#4443=CARTESIAN_POINT('Ctrl Pts',(-24.349705656948,0.405631974937107,-1.94411555901275));
#4444=CARTESIAN_POINT('Ctrl Pts',(-24.2778228093247,0.233283857786291,-1.97223255425957));
#4445=CARTESIAN_POINT('Ctrl Pts',(-24.2598233877886,0.139024680847256,-1.98118690809287));
#4446=CARTESIAN_POINT('Ctrl Pts',(-24.2598233877886,0.050000000000005,-1.9834311171324));
#4447=CARTESIAN_POINT('Ctrl Pts',(-24.6433379893901,0.674369275830048,-2.59955952546742));
#4448=CARTESIAN_POINT('Ctrl Pts',(-24.6590554485685,0.682336269919023,-2.59749275377718));
#4449=CARTESIAN_POINT('Ctrl Pts',(-24.6751102588048,0.689726977700771,-2.59553646483285));
#4450=CARTESIAN_POINT('Ctrl Pts',(-24.7775423290656,0.732251654012559,-2.58411714720213));
#4451=CARTESIAN_POINT('Ctrl Pts',(-24.8714588989999,0.750000000000003,-2.57875622086151));
#4452=CARTESIAN_POINT('Ctrl Pts',(-24.9598233877886,0.750000000000003,-2.57875622086151));
#4453=CARTESIAN_POINT('Origin',(-24.9598233877886,0.750000000000003,0.));
#4454=CARTESIAN_POINT('',(-26.9411105316953,0.750000000000003,2.57875622086151));
#4455=CARTESIAN_POINT('',(-24.9598233877886,0.750000000000003,2.57875622086151));
#4456=CARTESIAN_POINT('',(-25.7922242605427,0.750000000000003,2.57875622086151));
#4457=CARTESIAN_POINT('',(-26.9411105316953,0.750000000000003,1.83684484821366));
#4458=CARTESIAN_POINT('',(-26.9411105316953,0.750000000000003,-1.34280337788449));
#4459=CARTESIAN_POINT('',(-24.9598233877886,0.750000000000003,1.83684484821366));
#4460=CARTESIAN_POINT('',(-21.6665165759647,0.750000000000004,1.83684484821366));
#4461=CARTESIAN_POINT('',(-24.9598233877886,0.750000000000003,0.));
#4462=CARTESIAN_POINT('Origin',(-24.9598233877886,0.050000000000005,0.));
#4463=CARTESIAN_POINT('',(-24.6433379893901,0.674369275830023,2.59955952546743));
#4464=CARTESIAN_POINT('',(-24.2598233877886,0.0500000000000051,2.72441956476416));
#4465=CARTESIAN_POINT('Ctrl Pts',(-24.6433379893901,0.674369275830048,2.59955952546742));
#4466=CARTESIAN_POINT('Ctrl Pts',(-24.5948713345161,0.649802101930525,2.60593266180436));
#4467=CARTESIAN_POINT('Ctrl Pts',(-24.5496532706599,0.619791430299218,2.61528239730828));
#4468=CARTESIAN_POINT('Ctrl Pts',(-24.4417200371024,0.528744950462541,2.64346770524035));
#4469=CARTESIAN_POINT('Ctrl Pts',(-24.3860923106545,0.460462041863293,2.66434536458396));
#4470=CARTESIAN_POINT('Ctrl Pts',(-24.3090437545258,0.318322152326005,2.69712526693607));
#4471=CARTESIAN_POINT('Ctrl Pts',(-24.2840037138287,0.247396071480533,2.70974202041489));
#4472=CARTESIAN_POINT('Ctrl Pts',(-24.2634679001427,0.132431551146189,2.72119842129899));
#4473=CARTESIAN_POINT('Ctrl Pts',(-24.2598233877886,0.0912752037123824,
2.72366206022548));
#4474=CARTESIAN_POINT('Ctrl Pts',(-24.2598233877886,0.0500000000000052,
2.72441956476417));
#4475=CARTESIAN_POINT('Ctrl Pts',(-24.9598233877886,0.750000000000003,2.57875622086151));
#4476=CARTESIAN_POINT('Ctrl Pts',(-24.8714588989999,0.750000000000003,2.57875622086151));
#4477=CARTESIAN_POINT('Ctrl Pts',(-24.7775423290656,0.732251654012559,2.58411714720213));
#4478=CARTESIAN_POINT('Ctrl Pts',(-24.6751102588048,0.689726977700771,2.59553646483285));
#4479=CARTESIAN_POINT('Ctrl Pts',(-24.6590554485684,0.682336269919021,2.59749275377718));
#4480=CARTESIAN_POINT('Ctrl Pts',(-24.6433379893901,0.674369275830044,2.59955952546742));
#4481=CARTESIAN_POINT('',(-24.2598233877886,0.0500000000000051,1.9834311171324));
#4482=CARTESIAN_POINT('Ctrl Pts',(-24.2598233877886,0.050000000000005,1.9834311171324));
#4483=CARTESIAN_POINT('Ctrl Pts',(-24.2598233877886,0.139024680847256,1.98118690809287));
#4484=CARTESIAN_POINT('Ctrl Pts',(-24.2778228093247,0.233283857786291,1.97223255425957));
#4485=CARTESIAN_POINT('Ctrl Pts',(-24.349705656948,0.405631974937107,1.94411555901275));
#4486=CARTESIAN_POINT('Ctrl Pts',(-24.4035428766891,0.483787439248125,1.92524336790881));
#4487=CARTESIAN_POINT('Ctrl Pts',(-24.5269368573564,0.606943918256764,1.89002872240561));
#4488=CARTESIAN_POINT('Ctrl Pts',(-24.6049717534738,0.660537412507161,1.87126930464578));
#4489=CARTESIAN_POINT('Ctrl Pts',(-24.7769694082335,0.732084988974829,1.84445388640709));
#4490=CARTESIAN_POINT('Ctrl Pts',(-24.8710178004329,0.750000000000003,1.83684484821366));
#4491=CARTESIAN_POINT('Ctrl Pts',(-24.9598233877886,0.750000000000003,1.83684484821366));
#4492=CARTESIAN_POINT('',(-24.2598233877886,0.0500000000000051,0.));
#4493=CARTESIAN_POINT('Origin',(-24.2598233877886,-0.0499999999999985,0.));
#4494=CARTESIAN_POINT('',(-24.2598233877886,-3.33701353648822E-16,2.7248783394621));
#4495=CARTESIAN_POINT('Origin',(-24.2598233877886,0.,0.));
#4496=CARTESIAN_POINT('',(-24.2598233877886,-2.4297742445139E-16,1.9840612380693));
#4497=CARTESIAN_POINT('Origin',(-24.2598233877886,0.,0.));
#4498=CARTESIAN_POINT('',(-24.2598233877886,-0.0499999999999985,1.9834311171324));
#4499=CARTESIAN_POINT('Origin',(-24.2598233877886,0.,0.));
#4500=CARTESIAN_POINT('',(-24.2598233877886,-0.0499999999999985,2.72441956476416));
#4501=CARTESIAN_POINT('',(-24.2598233877886,-0.0499999999999985,0.));
#4502=CARTESIAN_POINT('Origin',(-24.2598233877886,0.,0.));
#4503=CARTESIAN_POINT('Origin',(-24.9598233877886,-0.0500000000000033,0.));
#4504=CARTESIAN_POINT('',(-24.6433379893901,-0.674369275830021,2.59955952546743));
#4505=CARTESIAN_POINT('Ctrl Pts',(-24.6433379893901,-0.674369275830042,
2.59955952546742));
#4506=CARTESIAN_POINT('Ctrl Pts',(-24.6590554485685,-0.682336269919019,
2.59749275377718));
#4507=CARTESIAN_POINT('Ctrl Pts',(-24.6751102588048,-0.689726977700767,
2.59553646483285));
#4508=CARTESIAN_POINT('Ctrl Pts',(-24.7775423290656,-0.732251654012554,
2.58411714720213));
#4509=CARTESIAN_POINT('Ctrl Pts',(-24.8714588989999,-0.749999999999997,
2.57875622086151));
#4510=CARTESIAN_POINT('Ctrl Pts',(-24.9598233877886,-0.749999999999997,
2.57875622086151));
#4511=CARTESIAN_POINT('Ctrl Pts',(-24.2598233877886,-0.0499999999999988,
2.72441956476417));
#4512=CARTESIAN_POINT('Ctrl Pts',(-24.2598233877886,-0.104924766187127,
2.72341155617956));
#4513=CARTESIAN_POINT('Ctrl Pts',(-24.2662698540133,-0.159426953545748,
2.71936770640943));
#4514=CARTESIAN_POINT('Ctrl Pts',(-24.2974260951431,-0.28987136967753,2.7030112297106));
#4515=CARTESIAN_POINT('Ctrl Pts',(-24.3286906053069,-0.36268639361365,2.68794464981024));
#4516=CARTESIAN_POINT('Ctrl Pts',(-24.4216661799565,-0.507384818705599,
2.65103909321305));
#4517=CARTESIAN_POINT('Ctrl Pts',(-24.4879327399939,-0.575597877337425,
2.62866780596057));
#4518=CARTESIAN_POINT('Ctrl Pts',(-24.5908215755151,-0.64559465234568,2.60749770242026));
#4519=CARTESIAN_POINT('Ctrl Pts',(-24.6166208950646,-0.660826696832337,
2.60307269725752));
#4520=CARTESIAN_POINT('Ctrl Pts',(-24.6433379893901,-0.674369275830043,
2.59955952546742));
#4521=CARTESIAN_POINT('Ctrl Pts',(-24.9598233877886,-0.749999999999997,
1.83684484821367));
#4522=CARTESIAN_POINT('Ctrl Pts',(-24.8710178004329,-0.749999999999997,
1.83684484821367));
#4523=CARTESIAN_POINT('Ctrl Pts',(-24.7769694082335,-0.732084988974822,
1.8444538864071));
#4524=CARTESIAN_POINT('Ctrl Pts',(-24.6049717534738,-0.660537412507153,
1.87126930464578));
#4525=CARTESIAN_POINT('Ctrl Pts',(-24.5269368573565,-0.606943918256759,
1.89002872240561));
#4526=CARTESIAN_POINT('Ctrl Pts',(-24.4035428766891,-0.483787439248121,
1.92524336790881));
#4527=CARTESIAN_POINT('Ctrl Pts',(-24.349705656948,-0.4056319749371,1.94411555901275));
#4528=CARTESIAN_POINT('Ctrl Pts',(-24.2778228093247,-0.233283857786286,
1.97223255425957));
#4529=CARTESIAN_POINT('Ctrl Pts',(-24.2598233877886,-0.139024680847255,
1.98118690809287));
#4530=CARTESIAN_POINT('Ctrl Pts',(-24.2598233877886,-0.0500000000000034,
1.9834311171324));
#4531=CARTESIAN_POINT('Origin',(-24.6433379893901,0.,0.));
#4532=CARTESIAN_POINT('',(-23.9997961170673,-3.42705006664759E-16,2.79839874569029));
#4533=CARTESIAN_POINT('Origin',(-23.9997961170673,0.,0.));
#4534=CARTESIAN_POINT('Origin',(-24.6433379893901,-5.60629501944673E-16,
4.57788729236058));
#4535=CARTESIAN_POINT('Origin',(-24.6433379893901,0.,0.));
#4536=CARTESIAN_POINT('Origin',(-24.6433379893901,0.,0.));
#4537=CARTESIAN_POINT('Origin',(-21.6665165759647,0.,0.));
#4538=CARTESIAN_POINT('',(-16.3919226202342,-2.4297742445139E-16,1.9840612380693));
#4539=CARTESIAN_POINT('',(-21.6665165759647,-2.4297742445139E-16,1.9840612380693));
#4540=CARTESIAN_POINT('Origin',(-16.3919226202342,0.,0.));
#4541=CARTESIAN_POINT('Origin',(-26.9411105316953,0.,0.));
#4542=CARTESIAN_POINT('Origin',(-26.9411105316953,0.,0.));
#4543=CARTESIAN_POINT('Origin',(-25.7922242605427,0.,0.));
#4544=CARTESIAN_POINT('Origin',(-26.9411105316953,0.,0.));
#4545=CARTESIAN_POINT('Origin',(-25.7922242605427,0.,0.));
#4546=CARTESIAN_POINT('Origin',(-26.9411105316953,0.,0.));
#4547=CARTESIAN_POINT('Origin',(-26.9411105316953,0.,-2.68560675576897));
#4548=CARTESIAN_POINT('Origin',(-26.9411105316953,0.,-2.68560675576897));
#4549=CARTESIAN_POINT('Origin',(-16.3919226202342,0.,-1.9840612380693));
#4550=CARTESIAN_POINT('',(-16.3919226202342,-2.83677232469619E-16,2.3164003912567));
#4551=CARTESIAN_POINT('Origin',(-16.3919226202342,0.,0.));
#4552=CARTESIAN_POINT('Origin',(-23.9374740777754,0.,0.));
#4553=CARTESIAN_POINT('',(-23.8751520384835,-3.42705006664759E-16,2.79839874569029));
#4554=CARTESIAN_POINT('Origin',(-23.8751520384835,0.,0.));
#4555=CARTESIAN_POINT('',(-23.9374740777754,-3.42705006664758E-16,2.79839874569029));
#4556=CARTESIAN_POINT('Origin',(-23.8146350180683,0.,0.));
#4557=CARTESIAN_POINT('',(-23.754117997653,-3.6746903553126E-16,3.00061238707443));
#4558=CARTESIAN_POINT('Origin',(-23.754117997653,0.,0.));
#4559=CARTESIAN_POINT('',(-23.8146350180683,-3.55087021098009E-16,2.89950556638236));
#4560=CARTESIAN_POINT('Origin',(-12.0843030466866,0.,0.));
#4561=CARTESIAN_POINT('',(-0.41448809572012,-3.6746903553126E-16,3.00061238707443));
#4562=CARTESIAN_POINT('Origin',(-0.41448809572012,0.,0.));
#4563=CARTESIAN_POINT('',(-12.0843030466866,-3.6746903553126E-16,3.00061238707443));
#4564=CARTESIAN_POINT('Origin',(-0.199995922856362,0.,0.));
#4565=CARTESIAN_POINT('',(0.0144962500073953,-3.57826880652553E-16,2.92187821747206));
#4566=CARTESIAN_POINT('',(-0.199995922856362,3.62647958091906E-16,2.96124530227324));
#4567=CARTESIAN_POINT('Origin',(0.0144962500073953,0.,0.));
#4568=CARTESIAN_POINT('Origin',(0.0144962500073953,0.,-2.3164003912567));
#4569=CARTESIAN_POINT('',(0.0144962500073953,-2.83677232469619E-16,2.3164003912567));
#4570=CARTESIAN_POINT('Origin',(0.0144962500073953,0.,0.));
#4571=CARTESIAN_POINT('Origin',(-8.1887131851134,0.,0.));
#4572=CARTESIAN_POINT('',(-8.1887131851134,-2.83677232469619E-16,2.3164003912567));
#4573=CARTESIAN_POINT('',(0.,0.,0.));
#4574=CARTESIAN_POINT('Origin',(-25.2637346688979,0.,2.35));
#4575=CARTESIAN_POINT('',(-25.8637346688979,-7.34788079488413E-17,2.3));
#4576=CARTESIAN_POINT('Origin',(-25.2637346688979,0.,2.3));
#4577=CARTESIAN_POINT('',(-25.7637346688979,6.1232339957368E-17,2.4));
#4578=CARTESIAN_POINT('',(-25.8137346688979,6.73555739531047E-17,2.35));
#4579=CARTESIAN_POINT('Origin',(-25.2637346688979,0.,2.4));
#4580=CARTESIAN_POINT('Origin',(-25.2637346688979,0.,0.));
#4581=CARTESIAN_POINT('',(-25.8637346688979,-7.34788079488413E-17,0.));
#4582=CARTESIAN_POINT('',(-25.8637346688979,-7.34788079488413E-17,0.));
#4583=CARTESIAN_POINT('Origin',(-25.2637346688979,0.,0.));
#4584=CARTESIAN_POINT('Origin',(-25.2637346688979,0.,2.4));
#4585=CARTESIAN_POINT('Origin',(-25.2637346688979,0.,0.));
#4586=CARTESIAN_POINT('',(0.,0.,0.));
#4587=CARTESIAN_POINT('',(0.,0.,0.));
#4588=CARTESIAN_POINT('',(0.,0.,0.));
#4589=CARTESIAN_POINT('',(0.,0.,0.));
#4590=CARTESIAN_POINT('',(0.,0.,0.));
#4591=CARTESIAN_POINT('',(0.,0.,0.));
#4592=CARTESIAN_POINT('',(0.,0.,0.));
#4593=CARTESIAN_POINT('',(0.,0.,0.));
#4594=UNCERTAINTY_MEASURE_WITH_UNIT(LENGTH_MEASURE(0.01),#4614,
'DISTANCE_ACCURACY_VALUE',
'Maximum model space distance between geometric entities at asserted c
onnectivities');
#4595=UNCERTAINTY_MEASURE_WITH_UNIT(LENGTH_MEASURE(0.01),#4614,
'DISTANCE_ACCURACY_VALUE',
'Maximum model space distance between geometric entities at asserted c
onnectivities');
#4596=UNCERTAINTY_MEASURE_WITH_UNIT(LENGTH_MEASURE(0.01),#4614,
'DISTANCE_ACCURACY_VALUE',
'Maximum model space distance between geometric entities at asserted c
onnectivities');
#4597=UNCERTAINTY_MEASURE_WITH_UNIT(LENGTH_MEASURE(0.01),#4614,
'DISTANCE_ACCURACY_VALUE',
'Maximum model space distance between geometric entities at asserted c
onnectivities');
#4598=UNCERTAINTY_MEASURE_WITH_UNIT(LENGTH_MEASURE(0.01),#4614,
'DISTANCE_ACCURACY_VALUE',
'Maximum model space distance between geometric entities at asserted c
onnectivities');
#4599=UNCERTAINTY_MEASURE_WITH_UNIT(LENGTH_MEASURE(0.01),#4614,
'DISTANCE_ACCURACY_VALUE',
'Maximum model space distance between geometric entities at asserted c
onnectivities');
#4600=UNCERTAINTY_MEASURE_WITH_UNIT(LENGTH_MEASURE(0.01),#4614,
'DISTANCE_ACCURACY_VALUE',
'Maximum model space distance between geometric entities at asserted c
onnectivities');
#4601=UNCERTAINTY_MEASURE_WITH_UNIT(LENGTH_MEASURE(0.01),#4614,
'DISTANCE_ACCURACY_VALUE',
'Maximum model space distance between geometric entities at asserted c
onnectivities');
#4602=UNCERTAINTY_MEASURE_WITH_UNIT(LENGTH_MEASURE(0.01),#4614,
'DISTANCE_ACCURACY_VALUE',
'Maximum model space distance between geometric entities at asserted c
onnectivities');
#4603=UNCERTAINTY_MEASURE_WITH_UNIT(LENGTH_MEASURE(0.01),#4614,
'DISTANCE_ACCURACY_VALUE',
'Maximum model space distance between geometric entities at asserted c
onnectivities');
#4604=(
GEOMETRIC_REPRESENTATION_CONTEXT(3)
GLOBAL_UNCERTAINTY_ASSIGNED_CONTEXT((#4594))
GLOBAL_UNIT_ASSIGNED_CONTEXT((#4614,#4616,#4617))
REPRESENTATION_CONTEXT('','3D')
);
#4605=(
GEOMETRIC_REPRESENTATION_CONTEXT(3)
GLOBAL_UNCERTAINTY_ASSIGNED_CONTEXT((#4595))
GLOBAL_UNIT_ASSIGNED_CONTEXT((#4614,#4616,#4617))
REPRESENTATION_CONTEXT('','3D')
);
#4606=(
GEOMETRIC_REPRESENTATION_CONTEXT(3)
GLOBAL_UNCERTAINTY_ASSIGNED_CONTEXT((#4596))
GLOBAL_UNIT_ASSIGNED_CONTEXT((#4614,#4616,#4617))
REPRESENTATION_CONTEXT('','3D')
);
#4607=(
GEOMETRIC_REPRESENTATION_CONTEXT(3)
GLOBAL_UNCERTAINTY_ASSIGNED_CONTEXT((#4597))
GLOBAL_UNIT_ASSIGNED_CONTEXT((#4614,#4616,#4617))
REPRESENTATION_CONTEXT('','3D')
);
#4608=(
GEOMETRIC_REPRESENTATION_CONTEXT(3)
GLOBAL_UNCERTAINTY_ASSIGNED_CONTEXT((#4598))
GLOBAL_UNIT_ASSIGNED_CONTEXT((#4614,#4616,#4617))
REPRESENTATION_CONTEXT('','3D')
);
#4609=(
GEOMETRIC_REPRESENTATION_CONTEXT(3)
GLOBAL_UNCERTAINTY_ASSIGNED_CONTEXT((#4599))
GLOBAL_UNIT_ASSIGNED_CONTEXT((#4614,#4616,#4617))
REPRESENTATION_CONTEXT('','3D')
);
#4610=(
GEOMETRIC_REPRESENTATION_CONTEXT(3)
GLOBAL_UNCERTAINTY_ASSIGNED_CONTEXT((#4600))
GLOBAL_UNIT_ASSIGNED_CONTEXT((#4614,#4616,#4617))
REPRESENTATION_CONTEXT('','3D')
);
#4611=(
GEOMETRIC_REPRESENTATION_CONTEXT(3)
GLOBAL_UNCERTAINTY_ASSIGNED_CONTEXT((#4601))
GLOBAL_UNIT_ASSIGNED_CONTEXT((#4614,#4616,#4617))
REPRESENTATION_CONTEXT('','3D')
);
#4612=(
GEOMETRIC_REPRESENTATION_CONTEXT(3)
GLOBAL_UNCERTAINTY_ASSIGNED_CONTEXT((#4602))
GLOBAL_UNIT_ASSIGNED_CONTEXT((#4614,#4616,#4617))
REPRESENTATION_CONTEXT('','3D')
);
#4613=(
GEOMETRIC_REPRESENTATION_CONTEXT(3)
GLOBAL_UNCERTAINTY_ASSIGNED_CONTEXT((#4603))
GLOBAL_UNIT_ASSIGNED_CONTEXT((#4614,#4616,#4617))
REPRESENTATION_CONTEXT('','3D')
);
#4614=(
LENGTH_UNIT()
NAMED_UNIT(*)
SI_UNIT(.MILLI.,.METRE.)
);
#4615=(
LENGTH_UNIT()
NAMED_UNIT(*)
SI_UNIT($,.METRE.)
);
#4616=(
NAMED_UNIT(*)
PLANE_ANGLE_UNIT()
SI_UNIT($,.RADIAN.)
);
#4617=(
NAMED_UNIT(*)
SI_UNIT($,.STERADIAN.)
SOLID_ANGLE_UNIT()
);
#4618=SHAPE_DEFINITION_REPRESENTATION(#4627,#4644);
#4619=SHAPE_DEFINITION_REPRESENTATION(#4628,#4645);
#4620=SHAPE_DEFINITION_REPRESENTATION(#4629,#4646);
#4621=SHAPE_DEFINITION_REPRESENTATION(#4630,#4647);
#4622=SHAPE_DEFINITION_REPRESENTATION(#4631,#4648);
#4623=SHAPE_DEFINITION_REPRESENTATION(#4632,#4649);
#4624=SHAPE_DEFINITION_REPRESENTATION(#4633,#4650);
#4625=SHAPE_DEFINITION_REPRESENTATION(#4634,#4651);
#4626=SHAPE_DEFINITION_REPRESENTATION(#4635,#4652);
#4627=PRODUCT_DEFINITION_SHAPE('',$,#4654);
#4628=PRODUCT_DEFINITION_SHAPE('',$,#4655);
#4629=PRODUCT_DEFINITION_SHAPE('',$,#4656);
#4630=PRODUCT_DEFINITION_SHAPE('',$,#4657);
#4631=PRODUCT_DEFINITION_SHAPE('',$,#4658);
#4632=PRODUCT_DEFINITION_SHAPE('',$,#4659);
#4633=PRODUCT_DEFINITION_SHAPE('',$,#4660);
#4634=PRODUCT_DEFINITION_SHAPE('',$,#4661);
#4635=PRODUCT_DEFINITION_SHAPE('',$,#4662);
#4636=PRODUCT_DEFINITION_SHAPE($,$,#35);
#4637=PRODUCT_DEFINITION_SHAPE($,$,#36);
#4638=PRODUCT_DEFINITION_SHAPE($,$,#37);
#4639=PRODUCT_DEFINITION_SHAPE($,$,#38);
#4640=PRODUCT_DEFINITION_SHAPE($,$,#39);
#4641=PRODUCT_DEFINITION_SHAPE($,$,#40);
#4642=PRODUCT_DEFINITION_SHAPE($,$,#41);
#4643=PRODUCT_DEFINITION_SHAPE($,$,#42);
#4644=SHAPE_REPRESENTATION('',(#1691,#1894,#1895,#1896,#1897,#1898,#1899,
#1900,#1901),#4604);
#4645=SHAPE_REPRESENTATION('',(#1692),#4605);
#4646=SHAPE_REPRESENTATION('',(#1695),#4606);
#4647=SHAPE_REPRESENTATION('',(#1728),#4607);
#4648=SHAPE_REPRESENTATION('',(#1765),#4608);
#4649=SHAPE_REPRESENTATION('',(#1791),#4609);
#4650=SHAPE_REPRESENTATION('',(#1812),#4610);
#4651=SHAPE_REPRESENTATION('',(#1841),#4611);
#4652=SHAPE_REPRESENTATION('',(#1886),#4612);
#4653=PRODUCT_DEFINITION_CONTEXT('part definition',#4682,'design');
#4654=PRODUCT_DEFINITION('BR-155','BR-155',#4663,#4653);
#4655=PRODUCT_DEFINITION('Ball','Ball',#4664,#4653);
#4656=PRODUCT_DEFINITION('Holder','Holder',#4665,#4653);
#4657=PRODUCT_DEFINITION('Knob','Knob',#4666,#4653);
#4658=PRODUCT_DEFINITION('Front_part','Front_part',#4667,#4653);
#4659=PRODUCT_DEFINITION('Back_part','Back_part',#4668,#4653);
#4660=PRODUCT_DEFINITION('Locker','Locker',#4669,#4653);
#4661=PRODUCT_DEFINITION('Adjustment_Part','Adjustment_Part',#4670,#4653);
#4662=PRODUCT_DEFINITION('Pin','Pin',#4671,#4653);
#4663=PRODUCT_DEFINITION_FORMATION('',$,#4684);
#4664=PRODUCT_DEFINITION_FORMATION('',$,#4685);
#4665=PRODUCT_DEFINITION_FORMATION('',$,#4686);
#4666=PRODUCT_DEFINITION_FORMATION('',$,#4687);
#4667=PRODUCT_DEFINITION_FORMATION('',$,#4688);
#4668=PRODUCT_DEFINITION_FORMATION('',$,#4689);
#4669=PRODUCT_DEFINITION_FORMATION('',$,#4690);
#4670=PRODUCT_DEFINITION_FORMATION('',$,#4691);
#4671=PRODUCT_DEFINITION_FORMATION('',$,#4692);
#4672=PRODUCT_RELATED_PRODUCT_CATEGORY('BR-155','BR-155',(#4684));
#4673=PRODUCT_RELATED_PRODUCT_CATEGORY('Ball','Ball',(#4685));
#4674=PRODUCT_RELATED_PRODUCT_CATEGORY('Holder','Holder',(#4686));
#4675=PRODUCT_RELATED_PRODUCT_CATEGORY('Knob','Knob',(#4687));
#4676=PRODUCT_RELATED_PRODUCT_CATEGORY('Front_part','Front_part',(#4688));
#4677=PRODUCT_RELATED_PRODUCT_CATEGORY('Back_part','Back_part',(#4689));
#4678=PRODUCT_RELATED_PRODUCT_CATEGORY('Locker','Locker',(#4690));
#4679=PRODUCT_RELATED_PRODUCT_CATEGORY('Adjustment_Part',
'Adjustment_Part',(#4691));
#4680=PRODUCT_RELATED_PRODUCT_CATEGORY('Pin','Pin',(#4692));
#4681=APPLICATION_PROTOCOL_DEFINITION('international standard',
'automotive_design',2009,#4682);
#4682=APPLICATION_CONTEXT(
'Core Data for Automotive Mechanical Design Process');
#4683=PRODUCT_CONTEXT('part definition',#4682,'mechanical');
#4684=PRODUCT('BR-155','BR-155',$,(#4683));
#4685=PRODUCT('Ball','Ball',$,(#4683));
#4686=PRODUCT('Holder','Holder',$,(#4683));
#4687=PRODUCT('Knob','Knob',$,(#4683));
#4688=PRODUCT('Front_part','Front_part',$,(#4683));
#4689=PRODUCT('Back_part','Back_part',$,(#4683));
#4690=PRODUCT('Locker','Locker',$,(#4683));
#4691=PRODUCT('Adjustment_Part','Adjustment_Part',$,(#4683));
#4692=PRODUCT('Pin','Pin',$,(#4683));
#4693=PRESENTATION_STYLE_ASSIGNMENT((#4698));
#4694=PRESENTATION_STYLE_ASSIGNMENT((#4699));
#4695=PRESENTATION_STYLE_ASSIGNMENT((#4700));
#4696=PRESENTATION_STYLE_ASSIGNMENT((#4701));
#4697=PRESENTATION_STYLE_ASSIGNMENT((#4702));
#4698=SURFACE_STYLE_USAGE(.BOTH.,#4703);
#4699=SURFACE_STYLE_USAGE(.BOTH.,#4704);
#4700=SURFACE_STYLE_USAGE(.BOTH.,#4705);
#4701=SURFACE_STYLE_USAGE(.BOTH.,#4706);
#4702=SURFACE_STYLE_USAGE(.BOTH.,#4707);
#4703=SURFACE_SIDE_STYLE('',(#4708));
#4704=SURFACE_SIDE_STYLE('',(#4709));
#4705=SURFACE_SIDE_STYLE('',(#4710));
#4706=SURFACE_SIDE_STYLE('',(#4711));
#4707=SURFACE_SIDE_STYLE('',(#4712));
#4708=SURFACE_STYLE_FILL_AREA(#4713);
#4709=SURFACE_STYLE_FILL_AREA(#4714);
#4710=SURFACE_STYLE_FILL_AREA(#4715);
#4711=SURFACE_STYLE_FILL_AREA(#4716);
#4712=SURFACE_STYLE_FILL_AREA(#4717);
#4713=FILL_AREA_STYLE('Steel - Satin',(#4718));
#4714=FILL_AREA_STYLE('Opaque(170,85,127)',(#4719));
#4715=FILL_AREA_STYLE('Opaque(255,255,255)',(#4720));
#4716=FILL_AREA_STYLE('Opaque(68,68,68)',(#4721));
#4717=FILL_AREA_STYLE('Opaque(160,160,160)',(#4722));
#4718=FILL_AREA_STYLE_COLOUR('Steel - Satin',#4723);
#4719=FILL_AREA_STYLE_COLOUR('Opaque(170,85,127)',#4724);
#4720=FILL_AREA_STYLE_COLOUR('Opaque(255,255,255)',#4725);
#4721=FILL_AREA_STYLE_COLOUR('Opaque(68,68,68)',#4726);
#4722=FILL_AREA_STYLE_COLOUR('Opaque(160,160,160)',#4727);
#4723=COLOUR_RGB('Steel - Satin', 0.09019608, 0.27058824, 0.51372549);
#4724=COLOUR_RGB('Opaque(170,85,127)', 0.09019608, 0.27058824, 0.51372549);
#4725=COLOUR_RGB('Opaque(255,255,255)', 0.66274510, 0.83137255, 0.94901961);
#4726=COLOUR_RGB('Opaque(68,68,68)', 0.31764706, 0.68627451, 0.89019608);
#4727=COLOUR_RGB('Opaque(160,160,160)', 0.66274510, 0.83137255, 0.94901961);
ENDSEC;
END-ISO-10303-21;
